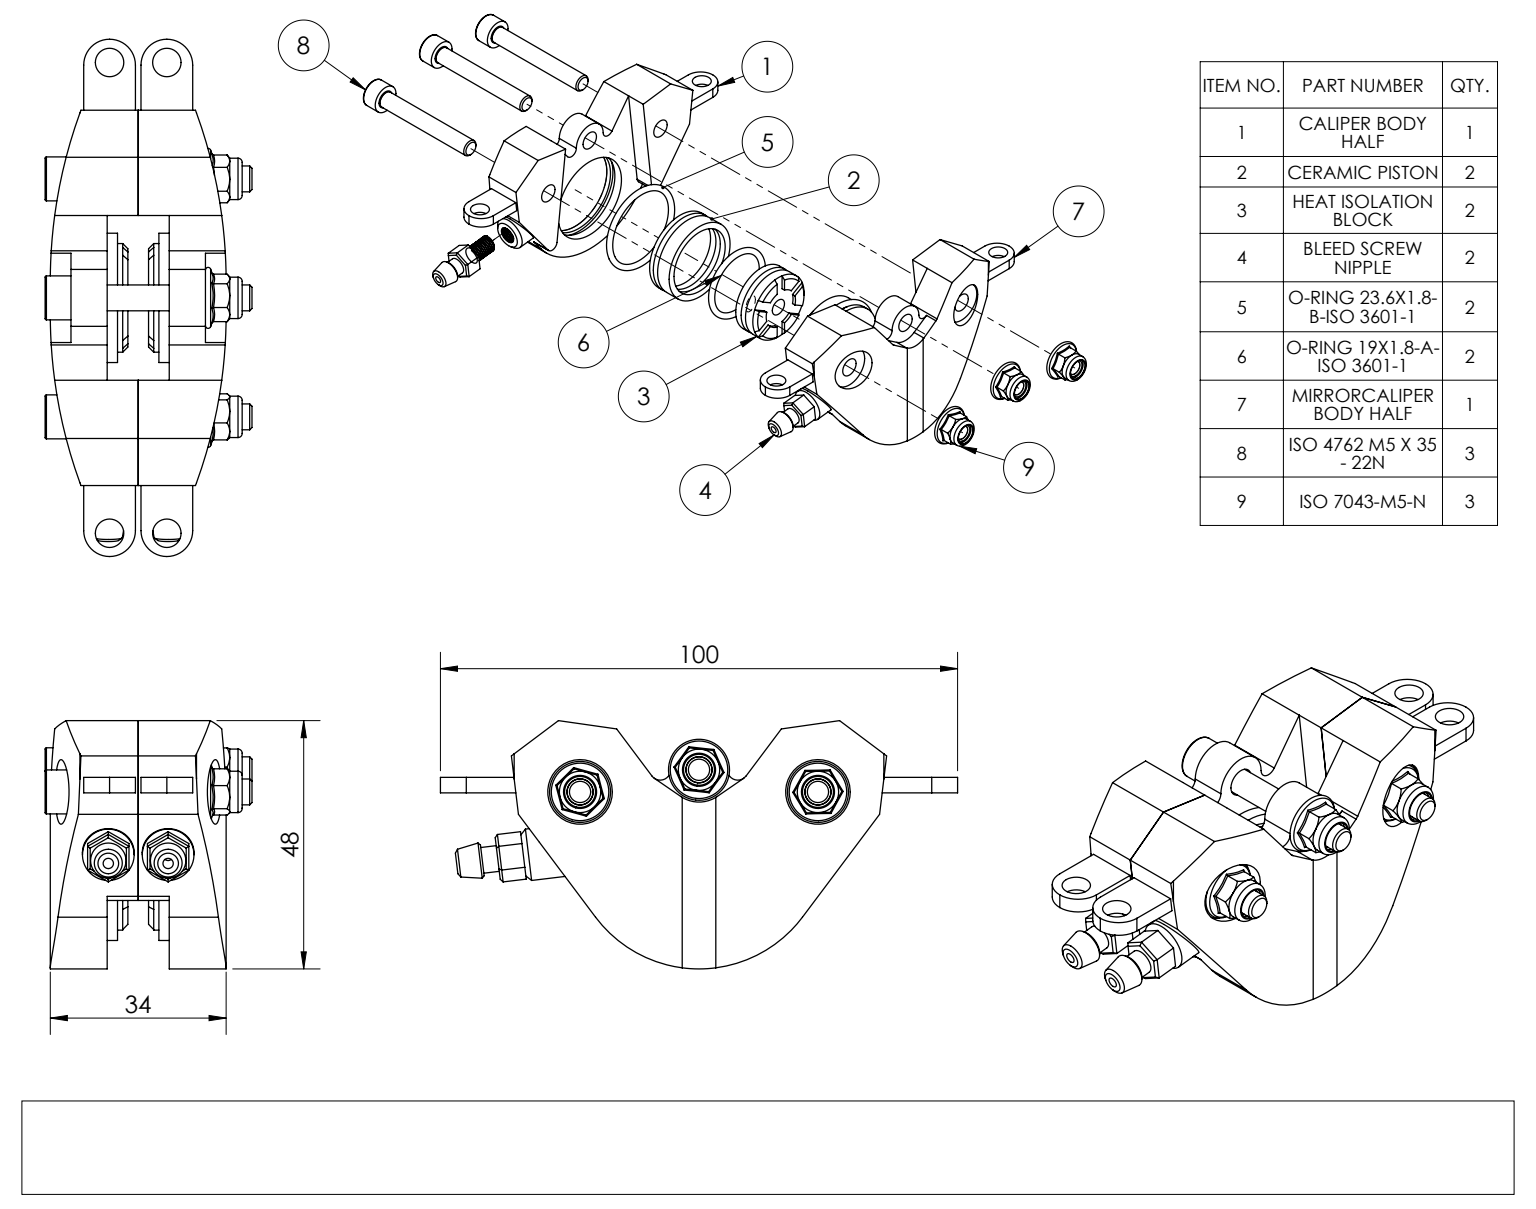
ISO-10303-21;
HEADER;
FILE_DESCRIPTION (('STEP AP214'),
    '1' );
FILE_NAME ('BR-592',
    '2026-09-24T10:28:59',
    ( '' ),
    ( '' ),
    'SwSTEP 2.0',
    'SolidWorks 2026',
    '' );
FILE_SCHEMA (( 'AUTOMOTIVE_DESIGN' ));
ENDSEC;

DATA;
#1 = DIRECTION ( 'NONE',  ( 0.000000000000000000, 0.000000000000000000, 1.000000000000000000 ) ) ;
#2 = CARTESIAN_POINT ( 'NONE',  ( 28.76238721243587193, -5.825490297734302381, -3.627061608673667781 ) ) ;
#3 = CARTESIAN_POINT ( 'NONE',  ( 28.60033944477555323, -4.591072787911525843, -8.283357778048662468 ) ) ;
#4 = FACE_OUTER_BOUND ( 'NONE', #16848, .T. ) ;
#5 = LINE ( 'NONE', #2469, #13948 ) ;
#6 = EDGE_CURVE ( 'NONE', #16160, #8560, #10428, .T. ) ;
#7 = CARTESIAN_POINT ( 'NONE',  ( 27.21934464581372737, -3.303641803799556964, -8.283357778048658915 ) ) ;
#8 = CARTESIAN_POINT ( 'NONE',  ( 31.38469755857769528, -2.374701023479507178, -4.705209693361161349 ) ) ;
#9 = CARTESIAN_POINT ( 'NONE',  ( -4.281152949374567029, -4.203775615332181914, -2.000000000000000000 ) ) ;
#10 = DIRECTION ( 'NONE',  ( -0.1196152422706611984, 0.9928203230275510771, 0.000000000000000000 ) ) ;
#11 = CARTESIAN_POINT ( 'NONE',  ( 0.5636734750061580534, 4.293365120987025385, -3.231543764079864101 ) ) ;
#12 = CARTESIAN_POINT ( 'NONE',  ( -4.140405595019059248, -2.228337868678524458, -3.386887224136967411 ) ) ;
#13 = VECTOR ( 'NONE', #4443, 1000.000000000000000 ) ;
#14 = EDGE_CURVE ( 'NONE', #9007, #1609, #16081, .T. ) ;
#15 =( GEOMETRIC_REPRESENTATION_CONTEXT ( 3 ) GLOBAL_UNCERTAINTY_ASSIGNED_CONTEXT ( ( #3731 ) ) GLOBAL_UNIT_ASSIGNED_CONTEXT ( ( #3713, #4977, #14697 ) ) REPRESENTATION_CONTEXT ( 'NONE', 'WORKASPACE' ) );
#16 = CARTESIAN_POINT ( 'NONE',  ( 29.62036837594175154, -3.214238380052812261, -3.627061608673662896 ) ) ;
#17 = EDGE_CURVE ( 'NONE', #16386, #12240, #657, .T. ) ;
#18 = ORIENTED_EDGE ( 'NONE', *, *, #8443, .T. ) ;
#19 = AXIS2_PLACEMENT_3D ( 'NONE', #16442, #1032, #9441 ) ;
#20 = CIRCLE ( 'NONE', #5504, 10.50000000000000000 ) ;
#21 = CARTESIAN_POINT ( 'NONE',  ( 32.63137222500256485, -6.623491938275930302, -6.453230759126470595 ) ) ;
#22 = CARTESIAN_POINT ( 'NONE',  ( 30.63309003953906995, -6.864245478665264244, -5.783357778048663356 ) ) ;
#23 = ORIENTED_EDGE ( 'NONE', *, *, #13213, .T. ) ;
#24 = DIRECTION ( 'NONE',  ( 0.000000000000000000, 0.000000000000000000, 1.000000000000000000 ) ) ;
#25 = ORIENTED_EDGE ( 'NONE', *, *, #5037, .F. ) ;
#26 = CARTESIAN_POINT ( 'NONE',  ( 30.41294626588012306, -6.253601060580800564, -6.861505862736167138 ) ) ;
#27 = EDGE_CURVE ( 'NONE', #7462, #10575, #2062, .T. ) ;
#28 = CYLINDRICAL_SURFACE ( 'NONE', #14824, 2.749999999999992006 ) ;
#29 = VERTEX_POINT ( 'NONE', #10521 ) ;
#30 = CARTESIAN_POINT ( 'NONE',  ( 26.73899421642883567, -2.634607751922174224, -4.533357778048659803 ) ) ;
#31 = VECTOR ( 'NONE', #7104, 1000.000000000000114 ) ;
#32 = CARTESIAN_POINT ( 'NONE',  ( 29.39961944441754227, -3.040961747597316744, 8.283357778048666020 ) ) ;
#33 = FACE_OUTER_BOUND ( 'NONE', #10742, .T. ) ;
#34 = CONICAL_SURFACE ( 'NONE', #10154, 3.500000000000004885, 0.1745329251994333364 ) ;
#35 = CARTESIAN_POINT ( 'NONE',  ( 26.41562710823574278, -3.600346414165641828, -7.939653947423660263 ) ) ;
#36 = EDGE_LOOP ( 'NONE', ( #1932, #7211, #3460, #1817 ) ) ;
#37 = CARTESIAN_POINT ( 'NONE',  ( 16.95685998530892746, -17.86641812890577796, -16.00584995567978908 ) ) ;
#38 = ORIENTED_EDGE ( 'NONE', *, *, #3823, .T. ) ;
#39 = CONICAL_SURFACE ( 'NONE', #2378, 9.500000000000001776, 0.7853981633974465026 ) ;
#40 = CARTESIAN_POINT ( 'NONE',  ( 27.63266882139180680, -2.199775856772564708, 5.783357778048668685 ) ) ;
#41 = CARTESIAN_POINT ( 'NONE',  ( 19.91592223102268733, -21.66952118561269458, 15.52717098632164117 ) ) ;
#42 = AXIS2_PLACEMENT_3D ( 'NONE', #3726, #1281, #2807 ) ;
#43 = VERTEX_POINT ( 'NONE', #14629 ) ;
#44 = VECTOR ( 'NONE', #8259, 1000.000000000000227 ) ;
#45 = CARTESIAN_POINT ( 'NONE',  ( 31.12210306526553083, -4.287250072544045665, 3.283357778048664244 ) ) ;
#46 = DIRECTION ( 'NONE',  ( 0.000000000000000000, 1.000000000000000000, 0.000000000000000000 ) ) ;
#47 = EDGE_CURVE ( 'NONE', #1330, #15856, #15716, .T. ) ;
#48 = ORIENTED_EDGE ( 'NONE', *, *, #12351, .T. ) ;
#49 = CARTESIAN_POINT ( 'NONE',  ( 33.55383270609817714, -5.448088258586239796, -3.283357778048667797 ) ) ;
#50 = CARTESIAN_POINT ( 'NONE',  ( 29.97942892559193950, -4.424919740341219487, -3.627061608673664672 ) ) ;
#51 = VECTOR ( 'NONE', #5337, 1000.000000000000000 ) ;
#52 = FACE_OUTER_BOUND ( 'NONE', #13800, .T. ) ;
#53 = CARTESIAN_POINT ( 'NONE',  ( -7.511572993685817836E-16, -4.618802153517020059, -3.133295621305386636 ) ) ;
#54 = PRESENTATION_STYLE_ASSIGNMENT (( #17863 ) ) ;
#55 = CARTESIAN_POINT ( 'NONE',  ( 0.000000000000000000, 0.000000000000000000, 0.000000000000000000 ) ) ;
#56 = CARTESIAN_POINT ( 'NONE',  ( 28.75786045390062995, -2.691183018653962034, 4.705209693361167567 ) ) ;
#57 = CARTESIAN_POINT ( 'NONE',  ( -15.92260893619738837, -28.39189527176317540, 12.00000000000000000 ) ) ;
#58 = CARTESIAN_POINT ( 'NONE',  ( 23.00000000000000000, -16.21813761408365195, 0.000000000000000000 ) ) ;
#59 = DIRECTION ( 'NONE',  ( 0.000000000000000000, 0.000000000000000000, 1.000000000000000000 ) ) ;
#60 = VERTEX_POINT ( 'NONE', #9170 ) ;
#61 = AXIS2_PLACEMENT_3D ( 'NONE', #16473, #4043, #10648 ) ;
#62 = CIRCLE ( 'NONE', #4991, 10.50000000000000000 ) ;
#63 = VERTEX_POINT ( 'NONE', #7643 ) ;
#64 = CARTESIAN_POINT ( 'NONE',  ( 27.60205212784272177, -2.830435096530727446, 6.861505862736165362 ) ) ;
#65 = CARTESIAN_POINT ( 'NONE',  ( 27.46709037723411839, -6.908327297984874882, 7.033357778048657138 ) ) ;
#66 = ORIENTED_EDGE ( 'NONE', *, *, #7774, .T. ) ;
#67 = CARTESIAN_POINT ( 'NONE',  ( 26.37178701114681800, -2.351687214456304797, 5.783357778048668685 ) ) ;
#68 = ORIENTED_EDGE ( 'NONE', *, *, #11555, .T. ) ;
#69 = DIRECTION ( 'NONE',  ( 0.5000000000000038858, 0.8660254037844363761, 0.000000000000000000 ) ) ;
#70 = CARTESIAN_POINT ( 'NONE',  ( 26.01652455409633902, -4.902371455920928156, -5.783357778048663356 ) ) ;
#71 = DIRECTION ( 'NONE',  ( 1.000000000000000000, 0.000000000000000000, 0.000000000000000000 ) ) ;
#72 = CARTESIAN_POINT ( 'NONE',  ( 25.86833963875586306, -3.039313213345869791, -4.705209693361160461 ) ) ;
#73 = CARTESIAN_POINT ( 'NONE',  ( 0.000000000000000000, 0.000000000000000000, -2.000000000000000000 ) ) ;
#75 = ADVANCED_FACE ( 'NONE', ( #15989 ), #17272, .F. ) ;
#74 = CARTESIAN_POINT ( 'NONE',  ( 29.12189622942009493, -1.620608325512071568, -5.783357778048658027 ) ) ;
#76 = CARTESIAN_POINT ( 'NONE',  ( 31.70371634254663817, -2.036456781249897485, -4.533357778048659803 ) ) ;
#77 = CIRCLE ( 'NONE', #17181, 2.000000000000001776 ) ;
#78 = CARTESIAN_POINT ( 'NONE',  ( 16.79147592569384173, -15.38964587861223166, -16.02981638571824163 ) ) ;
#79 = CARTESIAN_POINT ( 'NONE',  ( 30.08145424927873535, -6.930706697444451336, 5.783357778048664244 ) ) ;
#80 = CIRCLE ( 'NONE', #3851, 6.000000000000000888 ) ;
#81 = CARTESIAN_POINT ( 'NONE',  ( 29.62036837594175154, -3.214238380052812261, -3.627061608673662896 ) ) ;
#82 = VERTEX_POINT ( 'NONE', #13166 ) ;
#83 = EDGE_CURVE ( 'NONE', #825, #4804, #12452, .T. ) ;
#84 = CARTESIAN_POINT ( 'NONE',  ( 27.88665588685489993, -3.423116496867954162, -3.627061608673662008 ) ) ;
#85 = EDGE_LOOP ( 'NONE', ( #16844, #9736, #6237, #10207 ) ) ;
#86 = CARTESIAN_POINT ( 'NONE',  ( 0.000000000000000000, 0.000000000000000000, -4.700000000000000178 ) ) ;
#87 = EDGE_LOOP ( 'NONE', ( #1855, #1887, #10424, #16720 ) ) ;
#88 = ORIENTED_EDGE ( 'NONE', *, *, #6884, .F. ) ;
#89 = ORIENTED_EDGE ( 'NONE', *, *, #2806, .T. ) ;
#90 = CARTESIAN_POINT ( 'NONE',  ( 28.10549950023367316, -2.142809097641162897, 5.783357778048668685 ) ) ;
#91 = CARTESIAN_POINT ( 'NONE',  ( 26.87106449706838873, -6.053357334259913181, -3.627061608673667781 ) ) ;
#92 = DIRECTION ( 'NONE',  ( 0.000000000000000000, 0.000000000000000000, 1.000000000000000000 ) ) ;
#93 = CARTESIAN_POINT ( 'NONE',  ( 25.76466184735054910, -2.811881907026620553, -6.248149982130924762 ) ) ;
#94 = CARTESIAN_POINT ( 'NONE',  ( 34.91600907648203389, -11.88801210197604341, -11.56671555609732671 ) ) ;
#95 = CARTESIAN_POINT ( 'NONE',  ( 27.62849893492243325, -6.589071975465733644, -4.705209693361168455 ) ) ;
#96 = CARTESIAN_POINT ( 'NONE',  ( -4.000000000000000000, 2.309401076758501592, -0.4999999999999963363 ) ) ;
#97 = LINE ( 'NONE', #5605, #15979 ) ;
#98 = ADVANCED_FACE ( 'NONE', ( #4634, #14352 ), #12979, .F. ) ;
#99 = CARTESIAN_POINT ( 'NONE',  ( 25.11802603177690330, -16.03270077640482683, -0.5379818257722508434 ) ) ;
#100 = AXIS2_PLACEMENT_3D ( 'NONE', #12940, #16861, #525 ) ;
#101 = CARTESIAN_POINT ( 'NONE',  ( 28.51030546511822195, -6.055733689321201041, -3.283357778048667797 ) ) ;
#102 = AXIS2_PLACEMENT_3D ( 'NONE', #2745, #9523, #13625 ) ;
#103 = CARTESIAN_POINT ( 'NONE',  ( 30.62726312072365431, -1.838986382273682718, -5.783357778048658027 ) ) ;
#104 = CARTESIAN_POINT ( 'NONE',  ( 8.249999999999971578, -6.495190528383328221, -3.000000000000002665 ) ) ;
#105 = CARTESIAN_POINT ( 'NONE',  ( 31.03206908560819954, -5.751910973953721751, 8.283357778048660691 ) ) ;
#106 = EDGE_CURVE ( 'NONE', #16432, #2761, #668, .T. ) ;
#107 = DIRECTION ( 'NONE',  ( 0.000000000000000000, 0.000000000000000000, -1.000000000000000000 ) ) ;
#108 = CARTESIAN_POINT ( 'NONE',  ( 32.89331279191618762, -2.620040694222726785, 3.283357778048666464 ) ) ;
#109 = CARTESIAN_POINT ( 'NONE',  ( 26.84461768998868436, -2.294720455324902542, -5.783357778048658915 ) ) ;
#110 = ORIENTED_EDGE ( 'NONE', *, *, #14522, .T. ) ;
#111 = PLANE ( 'NONE',  #4436 ) ;
#112 = CARTESIAN_POINT ( 'NONE',  ( 0.000000000000000000, 0.000000000000000000, -4.000000000000000000 ) ) ;
#113 = ORIENTED_EDGE ( 'NONE', *, *, #12527, .T. ) ;
#114 = CARTESIAN_POINT ( 'NONE',  ( 31.97277696464621854, -6.702839660918840536, 5.783357778048664244 ) ) ;
#115 = ORIENTED_EDGE ( 'NONE', *, *, #562, .T. ) ;
#116 = CARTESIAN_POINT ( 'NONE',  ( 28.26310972651430120, -2.123820177930694442, -5.783357778048658915 ) ) ;
#117 = CARTESIAN_POINT ( 'NONE',  ( -23.02601376483258022, 3.965314980223224151, 6.000000000000000000 ) ) ;
#118 = VERTEX_POINT ( 'NONE', #924 ) ;
#119 = ORIENTED_EDGE ( 'NONE', *, *, #5679, .T. ) ;
#120 = CARTESIAN_POINT ( 'NONE',  ( 30.15026255541241440, -6.285249260098253465, -4.705209693361168455 ) ) ;
#121 = CARTESIAN_POINT ( 'NONE',  ( 29.19631194059803292, -2.001190877926593004, 6.453230759126469707 ) ) ;
#122 = VERTEX_POINT ( 'NONE', #5078 ) ;
#123 = CARTESIAN_POINT ( 'NONE',  ( 31.90644508241650357, -6.373472726347483963, -7.033357778048666908 ) ) ;
#124 = DIRECTION ( 'NONE',  ( 0.000000000000000000, 0.000000000000000000, -1.000000000000000000 ) ) ;
#125 = ORIENTED_EDGE ( 'NONE', *, *, #6084, .F. ) ;
#126 = CARTESIAN_POINT ( 'NONE',  ( 26.66770885555339987, -3.370103022578743612, 3.283357778048666464 ) ) ;
#127 = ADVANCED_FACE ( 'NONE', ( #4081 ), #12055, .F. ) ;
#128 = LINE ( 'NONE', #15357, #5139 ) ;
#129 = CARTESIAN_POINT ( 'NONE',  ( 27.17934203385504333, -30.00000000000000355, 0.000000000000000000 ) ) ;
#130 = DIRECTION ( 'NONE',  ( 0.8660254037844432595, 0.4999999999999921174, 0.000000000000000000 ) ) ;
#131 = VERTEX_POINT ( 'NONE', #5429 ) ;
#132 = CARTESIAN_POINT ( 'NONE',  ( 31.27600417729400917, -6.449428405189353342, 4.533357778048659803 ) ) ;
#133 = VERTEX_POINT ( 'NONE', #2641 ) ;
#134 = CARTESIAN_POINT ( 'NONE',  ( -3.248936832696171617, 7.999999999999989342, -17.00000000000000000 ) ) ;
#135 = ORIENTED_EDGE ( 'NONE', *, *, #7750, .F. ) ;
#136 = CARTESIAN_POINT ( 'NONE',  ( 0.000000000000000000, 0.000000000000000000, 0.000000000000000000 ) ) ;
#137 = EDGE_CURVE ( 'NONE', #13969, #14024, #12150, .T. ) ;
#138 = CARTESIAN_POINT ( 'NONE',  ( 27.02867472334902033, -6.034368414549446058, -3.627061608673668225 ) ) ;
#139 = CARTESIAN_POINT ( 'NONE',  ( 33.14105852333657509, -6.224726188408045147, -4.533357778048668685 ) ) ;
#140 = CARTESIAN_POINT ( 'NONE',  ( -2.016448651773435938E-27, -20.49999999999999645, -13.00000000000000178 ) ) ;
#141 = CARTESIAN_POINT ( 'NONE',  ( 31.03206908560819954, -5.751910973953721751, -3.283357778048667797 ) ) ;
#142 = CARTESIAN_POINT ( 'NONE',  ( 30.01874226414561875, -2.539271660970221944, 4.705209693361167567 ) ) ;
#143 = CARTESIAN_POINT ( 'NONE',  ( 0.000000000000000000, 0.000000000000000000, -3.000000000000000000 ) ) ;
#144 = CARTESIAN_POINT ( 'NONE',  ( 30.66050125466253107, -2.889050389913576655, -3.283357778048662023 ) ) ;
#145 = CARTESIAN_POINT ( 'NONE',  ( 31.55553118839817728, -4.235030543236534939, 3.627061608673664228 ) ) ;
#146 = ORIENTED_EDGE ( 'NONE', *, *, #8317, .T. ) ;
#147 = ADVANCED_FACE ( 'NONE', ( #12333 ), #17898, .T. ) ;
#148 = EDGE_LOOP ( 'NONE', ( #1703, #3321, #10614, #8753 ) ) ;
#149 = CARTESIAN_POINT ( 'NONE',  ( 28.24571643650507369, -4.633797857156355171, 3.627061608673664228 ) ) ;
#150 = CARTESIAN_POINT ( 'NONE',  ( 31.92138306490751987, -2.737139032229836566, -3.283357778048662023 ) ) ;
#151 = DIRECTION ( 'NONE',  ( 0.000000000000000000, 0.000000000000000000, -1.000000000000000000 ) ) ;
#152 = ORIENTED_EDGE ( 'NONE', *, *, #13921, .T. ) ;
#153 = CARTESIAN_POINT ( 'NONE',  ( 27.88665588685489993, -3.423116496867954162, 7.939653947423662927 ) ) ;
#154 = ORIENTED_EDGE ( 'NONE', *, *, #5892, .F. ) ;
#155 = ORIENTED_EDGE ( 'NONE', *, *, #14955, .F. ) ;
#156 = CYLINDRICAL_SURFACE ( 'NONE', #2297, 2.749999999999992006 ) ;
#157 = FACE_OUTER_BOUND ( 'NONE', #4677, .T. ) ;
#158 = DIRECTION ( 'NONE',  ( -1.000000000000000000, -0.000000000000000000, -0.000000000000000000 ) ) ;
#159 = B_SPLINE_CURVE_WITH_KNOTS ( 'NONE', 3,
 ( #17069, #3694, #6069, #7869 ),
 .UNSPECIFIED., .F., .F.,
 ( 4, 4 ),
 ( 0.000000000000000000, 0.0006487028241592422868 ),
 .UNSPECIFIED. ) ;
#160 = CARTESIAN_POINT ( 'NONE',  ( 26.52522735095806894, -6.721994413439005278, -4.705209693361169343 ) ) ;
#161 = CARTESIAN_POINT ( 'NONE',  ( 33.50243880635947846, -1.482387629897225390, -5.783357778048663356 ) ) ;
#162 = CARTESIAN_POINT ( 'NONE',  ( 27.92859066579839222, -3.218191664895003967, -8.283357778048658915 ) ) ;
#163 = CARTESIAN_POINT ( 'NONE',  ( 28.29479612530171551, -12.89112598890823946, -13.63906826012424922 ) ) ;
#164 = DIRECTION ( 'NONE',  ( 1.000000000000000000, 0.000000000000000000, 0.000000000000000000 ) ) ;
#165 =( LENGTH_UNIT ( ) NAMED_UNIT ( * ) SI_UNIT ( .MILLI., .METRE. ) );
#166 = CARTESIAN_POINT ( 'NONE',  ( 31.30154412293507349, -3.011689903141150815, -7.939653947423660263 ) ) ;
#167 = EDGE_LOOP ( 'NONE', ( #6855, #14181, #5684, #15430, #4604, #9201, #7856, #12095, #740, #13288, #12189, #5777, #2747, #13452, #12769, #7783, #17571, #8793, #8444, #8354, #17242, #15258, #14922, #10965, #8092, #5094, #9620, #17228, #363 ) ) ;
#168 = CARTESIAN_POINT ( 'NONE',  ( 28.28502977505876359, -2.748149777785362957, -6.861505862736158257 ) ) ;
#169 = FACE_BOUND ( 'NONE', #9729, .T. ) ;
#170 = ORIENTED_EDGE ( 'NONE', *, *, #10749, .T. ) ;
#171 = ORIENTED_EDGE ( 'NONE', *, *, #13786, .T. ) ;
#172 = VERTEX_POINT ( 'NONE', #5336 ) ;
#173 = ADVANCED_FACE ( 'NONE', ( #9510 ), #13344, .F. ) ;
#174 = ORIENTED_EDGE ( 'NONE', *, *, #13419, .F. ) ;
#175 = CARTESIAN_POINT ( 'NONE',  ( 30.04066231269008469, -3.163601260824890904, 3.627061608673666449 ) ) ;
#176 = CARTESIAN_POINT ( 'NONE',  ( 25.99795558426325215, -4.648046406214923820, -3.627061608673664228 ) ) ;
#177 = FACE_OUTER_BOUND ( 'NONE', #11097, .T. ) ;
#178 = DIRECTION ( 'NONE',  ( 0.000000000000000000, 0.000000000000000000, -1.000000000000000000 ) ) ;
#179 = CARTESIAN_POINT ( 'NONE',  ( 29.35841309260160159, -6.680460261459264970, -4.533357778048668685 ) ) ;
#180 = CARTESIAN_POINT ( 'NONE',  ( 29.51982165028991645, -6.361204938940122844, -4.705209693361168455 ) ) ;
#181 = CARTESIAN_POINT ( 'NONE',  ( 31.97277696464621854, -6.702839660918840536, -5.783357778048663356 ) ) ;
#182 = EDGE_CURVE ( 'NONE', #5342, #17048, #16351, .T. ) ;
#183 = DIRECTION ( 'NONE',  ( 1.000000000000000000, 0.000000000000000000, 0.000000000000000000 ) ) ;
#184 = ORIENTED_EDGE ( 'NONE', *, *, #3114, .F. ) ;
#185 = CARTESIAN_POINT ( 'NONE',  ( -27.17934203385504333, -30.00000000000000355, -13.93658524716016878 ) ) ;
#186 = CARTESIAN_POINT ( 'NONE',  ( 29.18195272205665347, -2.340279496617377664, -4.533357778048659803 ) ) ;
#187 =( BOUNDED_SURFACE ( )  B_SPLINE_SURFACE ( 3, 2, ( 
 ( #15565, #5853, #6132 ),
 ( #7149, #10017, #8682 ),
 ( #15660, #7420, #17130 ),
 ( #8776, #4680, #7501 ),
 ( #518, #1619, #4589 ),
 ( #14209, #7333, #249 ) ),
 .UNSPECIFIED., .F., .F., .T. ) 
 B_SPLINE_SURFACE_WITH_KNOTS ( ( 4, 2, 4 ),
 ( 3, 3 ),
 ( 0.02018906359535397113, 0.02264947622839649788, 0.02510988886143902810 ),
 ( 0.000000000000000000, 1.000000000000000000 ),
 .UNSPECIFIED. ) 
 GEOMETRIC_REPRESENTATION_ITEM ( )  RATIONAL_B_SPLINE_SURFACE ( (
 ( 1.000000000000000000, 0.8047781357041529082, 1.000000000000000000),
 ( 1.000000000000000000, 0.8123775905861528868, 1.000000000000000000),
 ( 1.000000000000000000, 0.8190671519372876297, 1.000000000000000000),
 ( 1.000000000000000000, 0.8192352278312100555, 1.000000000000000000),
 ( 1.000000000000000000, 0.8126131206996280998, 1.000000000000000000),
 ( 1.000000000000000000, 0.8047712494894333490, 1.000000000000000000) ) ) 
 REPRESENTATION_ITEM ( '' )  SURFACE ( )  );
#188 = CARTESIAN_POINT ( 'NONE',  ( 31.41114436565740320, -6.133337902414513820, -4.705209693361168455 ) ) ;
#189 = FACE_OUTER_BOUND ( 'NONE', #16988, .T. ) ;
#190 = DIRECTION ( 'NONE',  ( -1.000000000000000000, 0.000000000000000000, 0.000000000000000000 ) ) ;
#191 = CARTESIAN_POINT ( 'NONE',  ( 39.34669483983374505, -6.862522726337943801, -6.650911402496568314 ) ) ;
#192 = CARTESIAN_POINT ( 'NONE',  ( 31.59864285835955400, -2.049116061056871274, 4.533357778048667797 ) ) ;
#193 = CARTESIAN_POINT ( 'NONE',  ( 27.60205212784272177, -2.830435096530727446, -4.705209693361161349 ) ) ;
#194 = EDGE_CURVE ( 'NONE', #11172, #2496, #13438, .T. ) ;
#195 = ORIENTED_EDGE ( 'NONE', *, *, #15251, .T. ) ;
#196 = CARTESIAN_POINT ( 'NONE',  ( 26.87859896403794835, -7.316587507915443211, 5.113484796970851676 ) ) ;
#197 = DIRECTION ( 'NONE',  ( -1.000000000000000000, 0.000000000000000000, 0.000000000000000000 ) ) ;
#198 = ORIENTED_EDGE ( 'NONE', *, *, #5351, .T. ) ;
#199 = DIRECTION ( 'NONE',  ( 0.000000000000000000, -1.000000000000000000, 0.000000000000000000 ) ) ;
#200 = EDGE_LOOP ( 'NONE', ( #3718, #1302, #8199, #7677, #6005, #1633 ) ) ;
#201 = EDGE_CURVE ( 'NONE', #3274, #13752, #311, .T. ) ;
#202 = DIRECTION ( 'NONE',  ( -1.000000000000000000, 0.000000000000000000, 0.000000000000000000 ) ) ;
#203 = CARTESIAN_POINT ( 'NONE',  ( 3.248936832696173393, 17.78798921770683350, 17.00000000000000000 ) ) ;
#204 = ORIENTED_EDGE ( 'NONE', *, *, #11417, .T. ) ;
#205 = VECTOR ( 'NONE', #5367, 1000.000000000000227 ) ;
#207 = EDGE_LOOP ( 'NONE', ( #11422, #8377, #17595, #13814 ) ) ;
#206 =( BOUNDED_CURVE ( )  B_SPLINE_CURVE ( 2, ( #6130, #9128, #12848, #438, #15840, #5943, #14486, #14392, #13119 ),
 .UNSPECIFIED., .F., .T. ) 
 B_SPLINE_CURVE_WITH_KNOTS ( ( 3, 2, 2, 2, 3 ),
 ( 0.6730769230769231282, 0.6794871794871795156, 0.6923076923076922906, 0.7051282051282051766, 0.7115384615384615641 ),
 .UNSPECIFIED. ) 
 CURVE ( )  GEOMETRIC_REPRESENTATION_ITEM ( )  RATIONAL_B_SPLINE_CURVE ( ( 0.9330127018922192983, 0.9330127018922198534, 1.000000000000000000, 0.8660254037844387076, 1.000000000000000000, 0.8660254037844387076, 1.000000000000000000, 0.9330127018922194093, 0.9330127018922194093 ) ) 
 REPRESENTATION_ITEM ( '' )  );
#208 = CARTESIAN_POINT ( 'NONE',  ( 28.86293393808771057, -2.678523738846987357, -4.705209693361161349 ) ) ;
#209 = CARTESIAN_POINT ( 'NONE',  ( 42.20068782821381603, -5.470578387159230616, -5.783357778048662468 ) ) ;
#210 = CARTESIAN_POINT ( 'NONE',  ( 32.57506351453486815, -6.630276025878011126, 6.453230759126467042 ) ) ;
#211 = ORIENTED_EDGE ( 'NONE', *, *, #16657, .F. ) ;
#212 = CARTESIAN_POINT ( 'NONE',  ( 33.55383270609817714, -5.448088258586239796, -3.283357778048667797 ) ) ;
#213 = ORIENTED_EDGE ( 'NONE', *, *, #17178, .T. ) ;
#214 = CARTESIAN_POINT ( 'NONE',  ( 31.61111609099199171, -1.710254666422835745, -5.783357778048662468 ) ) ;
#215 = CARTESIAN_POINT ( 'NONE',  ( 33.17547354829333273, -5.293800545841212291, 7.939653947423658487 ) ) ;
#216 = AXIS2_PLACEMENT_3D ( 'NONE', #2816, #4451, #10954 ) ;
#217 = AXIS2_PLACEMENT_3D ( 'NONE', #13648, #13735, #1318 ) ;
#218 = EDGE_CURVE ( 'NONE', #17680, #17749, #13335, .T. ) ;
#219 = VECTOR ( 'NONE', #12447, 1000.000000000000000 ) ;
#220 = DIRECTION ( 'NONE',  ( 0.9928203230275512992, 0.1196152422706610319, 9.614813431917826478E-17 ) ) ;
#221 = DIRECTION ( 'NONE',  ( 0.9899494936611662466, -0.1414213562373111965, 0.000000000000000000 ) ) ;
#222 = CARTESIAN_POINT ( 'NONE',  ( -25.11802603177690330, -19.03270077640482683, -10.53798182577225084 ) ) ;
#223 = ORIENTED_EDGE ( 'NONE', *, *, #9237, .T. ) ;
#224 = CARTESIAN_POINT ( 'NONE',  ( 28.67914455963771303, -4.581578327848842669, 3.283357778048664244 ) ) ;
#225 = VERTEX_POINT ( 'NONE', #1017 ) ;
#226 = CARTESIAN_POINT ( 'NONE',  ( 26.92924972366625980, -7.310485091653801781, 5.783357778048669573 ) ) ;
#227 = VERTEX_POINT ( 'NONE', #1284 ) ;
#228 = CARTESIAN_POINT ( 'NONE',  ( 45.50000000000000000, -16.03270077640482683, 5.537981825772250843 ) ) ;
#229 = CARTESIAN_POINT ( 'NONE',  ( 25.93488947238681774, -5.606027099510431988, -7.939653947423663816 ) ) ;
#230 = ADVANCED_FACE ( 'NONE', ( #6542 ), #5163, .T. ) ;
#231 = CARTESIAN_POINT ( 'NONE',  ( 31.74131510559286085, -5.666460835049168310, -3.283357778048667797 ) ) ;
#232 = DIRECTION ( 'NONE',  ( 0.000000000000000000, 0.000000000000000000, -1.000000000000000000 ) ) ;
#233 = APPLICATION_PROTOCOL_DEFINITION ( 'draft international standard', 'automotive_design', 1998, #5728 ) ;
#234 = DIRECTION ( 'NONE',  ( 1.000000000000000000, 0.000000000000000000, 0.000000000000000000 ) ) ;
#235 =( GEOMETRIC_REPRESENTATION_CONTEXT ( 3 ) GLOBAL_UNCERTAINTY_ASSIGNED_CONTEXT ( ( #1389 ) ) GLOBAL_UNIT_ASSIGNED_CONTEXT ( ( #897, #4698, #14414 ) ) REPRESENTATION_CONTEXT ( 'NONE', 'WORKASPACE' ) );
#236 = DIRECTION ( 'NONE',  ( 0.000000000000000000, 0.000000000000000000, 1.000000000000000000 ) ) ;
#237 = CARTESIAN_POINT ( 'NONE',  ( 31.70371634254663817, -2.036456781249897485, 7.033357778048666020 ) ) ;
#238 = CARTESIAN_POINT ( 'NONE',  ( 29.52399153675929355, -1.971908820246954130, 5.783357778048668685 ) ) ;
#239 = ORIENTED_EDGE ( 'NONE', *, *, #8844, .T. ) ;
#240 = VECTOR ( 'NONE', #8984, 1000.000000000000000 ) ;
#241 = ORIENTED_EDGE ( 'NONE', *, *, #27, .F. ) ;
#242 = CARTESIAN_POINT ( 'NONE',  ( 29.49337484321020497, -2.602568060005117090, 6.861505862736165362 ) ) ;
#243 = DIRECTION ( 'NONE',  ( 0.000000000000000000, 0.000000000000000000, -1.000000000000000000 ) ) ;
#244 = CARTESIAN_POINT ( 'NONE',  ( 26.00347982711925710, -2.723222710571018279, -7.033357778048658027 ) ) ;
#245 = ORIENTED_EDGE ( 'NONE', *, *, #2656, .T. ) ;
#246 = CARTESIAN_POINT ( 'NONE',  ( 27.12922144900085186, -2.887401855662130146, 6.861505862736166250 ) ) ;
#247 = DIRECTION ( 'NONE',  ( -0.9928203230275512992, -0.1196152422706610319, -9.614813431917826478E-17 ) ) ;
#248 = AXIS2_PLACEMENT_3D ( 'NONE', #3421, #10388, #11749 ) ;
#249 = CARTESIAN_POINT ( 'NONE',  ( -4.211405941597130109, -2.460460478483078361, -3.451298436431160077 ) ) ;
#250 = CARTESIAN_POINT ( 'NONE',  ( 0.000000000000000000, 0.000000000000000000, -9.600000000000001421 ) ) ;
#251 = CIRCLE ( 'NONE', #10368, 10.50000000000000000 ) ;
#252 = CYLINDRICAL_SURFACE ( 'NONE', #8155, 1.000000000000000000 ) ;
#253 = CARTESIAN_POINT ( 'NONE',  ( 0.000000000000000000, 0.000000000000000000, -9.600000000000001421 ) ) ;
#254 = VERTEX_POINT ( 'NONE', #16603 ) ;
#255 = CARTESIAN_POINT ( 'NONE',  ( 31.11087420047036289, -5.742416513891037688, -3.283357778048667797 ) ) ;
#256 = ADVANCED_FACE ( 'NONE', ( #8427, #1643 ), #16881, .T. ) ;
#257 = CARTESIAN_POINT ( 'NONE',  ( 19.43845002722867221, 2.988003976273735596, -6.000000000000000000 ) ) ;
#258 = CARTESIAN_POINT ( 'NONE',  ( 0.000000000000000000, 0.000000000000000000, -4.394516984716110741 ) ) ;
#259 = APPLICATION_PROTOCOL_DEFINITION ( 'draft international standard', 'automotive_design', 1998, #17836 ) ;
#260 = CARTESIAN_POINT ( 'NONE',  ( 32.77257290155422709, -2.834459985843461816, -3.627061608673662896 ) ) ;
#261 = VECTOR ( 'NONE', #7073, 1000.000000000000227 ) ;
#262 = CARTESIAN_POINT ( 'NONE',  ( 25.76466184735054910, -2.811881907026620553, -6.248149982130924762 ) ) ;
#263 = CARTESIAN_POINT ( 'NONE',  ( -9.099998387031003944, -19.29508120620799616, -16.81964500401478091 ) ) ;
#264 = CIRCLE ( 'NONE', #10381, 4.250000000000000000 ) ;
#265 = EDGE_CURVE ( 'NONE', #1659, #12087, #14509, .T. ) ;
#266 = ORIENTED_EDGE ( 'NONE', *, *, #8133, .F. ) ;
#267 = EDGE_LOOP ( 'NONE', ( #17915, #6076 ) ) ;
#268 = CARTESIAN_POINT ( 'NONE',  ( 27.75549246765397271, -7.200742295513424374, 5.783357778048658915 ) ) ;
#269 = DIRECTION ( 'NONE',  ( -0.1196152422706618645, 0.9928203230275510771, 0.000000000000000000 ) ) ;
#270 = CARTESIAN_POINT ( 'NONE',  ( 23.00000000000000000, -16.21813761408365195, -13.00000000000000178 ) ) ;
#271 = PLANE ( 'NONE',  #2587 ) ;
#272 = CARTESIAN_POINT ( 'NONE',  ( 0.000000000000000000, -1.178949249685218081, -2.041999999999998039 ) ) ;
#273 = CARTESIAN_POINT ( 'NONE',  ( 30.04066231269008469, -3.163601260824890904, -7.939653947423660263 ) ) ;
#274 = CARTESIAN_POINT ( 'NONE',  ( 29.26075783691881682, -2.330785036554694489, -4.533357778048659803 ) ) ;
#275 = CARTESIAN_POINT ( 'NONE',  ( 26.01652455409633902, -4.902371455920926380, -5.783357778048663356 ) ) ;
#276 = VECTOR ( 'NONE', #9402, 1000.000000000000227 ) ;
#277 = LINE ( 'NONE', #4351, #8745 ) ;
#278 = EDGE_CURVE ( 'NONE', #1298, #15606, #15319, .T. ) ;
#279 = UNCERTAINTY_MEASURE_WITH_UNIT (LENGTH_MEASURE( 1.000000000000000082E-05 ), #1494, 'distance_accuracy_value', 'NONE');
#280 = CARTESIAN_POINT ( 'NONE',  ( 5.200000000000002842, 0.000000000000000000, 2.500000000000000444 ) ) ;
#281 = ORIENTED_EDGE ( 'NONE', *, *, #15299, .F. ) ;
#282 = CARTESIAN_POINT ( 'NONE',  ( 28.88938074516742205, -6.437160617781993999, -4.705209693361168455 ) ) ;
#283 = LINE ( 'NONE', #14248, #9848 ) ;
#284 = DIRECTION ( 'NONE',  ( 0.9899494936611662466, -0.1414213562373111965, 0.000000000000000000 ) ) ;
#285 = CARTESIAN_POINT ( 'NONE',  ( -15.92260893619738837, -28.39189527176317540, 16.15082599432113142 ) ) ;
#286 = VECTOR ( 'NONE', #8460, 1000.000000000000227 ) ;
#287 = DIRECTION ( 'NONE',  ( -0.1196152422706621005, -0.9928203230275509661, 0.000000000000000000 ) ) ;
#288 = CARTESIAN_POINT ( 'NONE',  ( 31.94023320572814484, -7.096308717197083560, 5.783357778048657138 ) ) ;
#289 = CARTESIAN_POINT ( 'NONE',  ( 26.35439372113758694, -4.861664893681965083, -7.939653947423662039 ) ) ;
#290 = VECTOR ( 'NONE', #14393, 1000.000000000000000 ) ;
#291 = ORIENTED_EDGE ( 'NONE', *, *, #11495, .T. ) ;
#292 = CARTESIAN_POINT ( 'NONE',  ( -35.77680296528374271, -19.03270077640482683, -10.53798182577225084 ) ) ;
#293 = DIRECTION ( 'NONE',  ( 0.9237280213470681067, 0.3830490080632377170, 0.000000000000000000 ) ) ;
#294 = CARTESIAN_POINT ( 'NONE',  ( -19.22778933661430756, -11.21824206523807099, -15.64718775662042560 ) ) ;
#295 = ORIENTED_EDGE ( 'NONE', *, *, #12061, .T. ) ;
#296 = AXIS2_PLACEMENT_3D ( 'NONE', #16194, #10362, #13007 ) ;
#297 =( BOUNDED_SURFACE ( )  B_SPLINE_SURFACE ( 1, 2, ( 
 ( #2861, #15197, #16560, #1329, #12111, #15107, #10908, #4144, #1250, #8037, #10736, #5570, #5480, #9559, #4046, #9474, #17694, #15013, #3878, #2779, #5217, #13662, #9391, #13829, #1416, #14933, #6939, #11088, #13573, #1154, #6676, #12207, #5305, #10826, #2693, #336, #16742, #6022, #9824, #15375, #8767, #5843, #145, #12649, #14022, #4493, #11547, #11262, #1693, #12921, #5748, #3051, #11366, #3136, #7410, #11170, #4404, #1607, #15648, #4314, #16935, #8571, #10007, #14299, #2958, #428, #5933, #1884, #506, #17116, #12739, #4670, #7137, #8487, #15553, #238, #8669, #16841, #5659, #12840, #9919, #14106, #12564, #15469, #11457, #10197, #7226, #15747, #8388, #13920, #14196, #1790, #1516, #17024, #7321, #4578, #10099, #3226, #7049, #17304, #13377, #9199, #6214, #9119, #17215, #7674, #3496, #14476, #4756, #13013, #6492, #10628, #863, #6120, #2156, #13284, #15921, #11732, #7583, #2060, #11648, #10465, #12006, #10281, #14658, #17588, #690, #17503, #15830, #13198, #959, #6395, #2240, #7753, #16026, #11913, #598, #5108, #4841, #7490, #2331, #5027, #3403, #3598, #10549, #7850, #16113, #9026, #3675, #10369, #14577, #14745, #8935, #13110, #775 ),
 ( #8849, #3320, #6302, #11824, #14384, #1966, #17402, #4932, #6566, #5194, #5614, #8440, #5799, #12613, #1562, #11131, #7186, #108, #9454, #13976, #3940, #10715, #13473, #6652, #12182, #1466, #13879, #15330, #11219, #12086, #6994, #16288, #1046, #2491, #3858, #14991, #12696, #2908, #9777, #3012, #192, #9368, #5704, #17673, #9287, #288, #2578, #13552, #4274, #16201, #14909, #7095, #3766, #8014, #14829, #1127, #8347, #17761, #5284, #2414, #16794, #7936, #15427, #12522, #16700, #10801, #16376, #4362, #9872, #14068, #8534, #1651, #4454, #14150, #385, #556, #3281, #14252, #11695, #8897, #1840, #11603, #5893, #10323, #12789, #11315, #17073, #3455, #8813, #16895, #12973, #3180, #17167, #15515, #7370, #13155, #3097, #5977, #14344, #7274, #11414, #6074, #8620, #8985, #4716, #16980, #14528, #7450, #10150, #12886, #2111, #471, #1744, #15790, #735, #11502, #9965, #14430, #6171, #4535, #3365, #17264, #15880, #10055, #7539, #15604, #10242, #2014, #8720, #1931, #4626, #7634, #15700, #13064, #4800, #647, #15980, #10512, #11874, #2379, #3903, #9164, #17550, #10763, #3642, #916, #16157, #1010, #5243, #9079, #2286, #17452, #13517, #14621, #3721 ) ),
 .UNSPECIFIED., .F., .F., .F. ) 
 B_SPLINE_SURFACE_WITH_KNOTS ( ( 2, 2 ),
 ( 3, 2, 2, 2, 2, 2, 2, 2, 2, 2, 2, 2, 2, 2, 2, 2, 2, 2, 2, 2, 2, 2, 2, 2, 2, 2, 2, 2, 2, 2, 2, 2, 2, 2, 2, 2, 2, 2, 2, 2, 2, 2, 2, 2, 2, 2, 2, 2, 2, 2, 2, 2, 2, 2, 2, 2, 2, 2, 2, 2, 2, 2, 2, 2, 2, 2, 2, 2, 2, 2, 2, 2, 2, 2, 2, 2, 2, 3 ),
 ( 0.000000000000000000, 1.000000000000000000 ),
 ( 0.000000000000000000, 0.01282051282051282007, 0.02564102564102564014, 0.03846153846153846367, 0.05128205128205128027, 0.06410256410256409687, 0.07692307692307692735, 0.08974358974358974395, 0.1025641025641025605, 0.1153846153846153910, 0.1282051282051281937, 0.1410256410256410242, 0.1538461538461538547, 0.1666666666666666574, 0.1794871794871794879, 0.1923076923076923184, 0.2051282051282051211, 0.2179487179487179516, 0.2307692307692307820, 0.2435897435897435848, 0.2564102564102563875, 0.2692307692307692180, 0.2820512820512820484, 0.2948717948717948789, 0.3076923076923077094, 0.3205128205128205399, 0.3333333333333333148, 0.3461538461538461453, 0.3589743589743589758, 0.3717948717948718063, 0.3846153846153846367, 0.3974358974358974117, 0.4102564102564102422, 0.4230769230769230727, 0.4358974358974359031, 0.4487179487179487336, 0.4615384615384615641, 0.4743589743589743390, 0.4871794871794871695, 0.5000000000000000000, 0.5128205128205127750, 0.5256410256410256610, 0.5384615384615384359, 0.5512820512820513219, 0.5641025641025640969, 0.5769230769230768718, 0.5897435897435897578, 0.6025641025641025328, 0.6153846153846154188, 0.6282051282051281937, 0.6410256410256410797, 0.6538461538461538547, 0.6666666666666666297, 0.6794871794871795156, 0.6923076923076922906, 0.7051282051282051766, 0.7179487179487179516, 0.7307692307692307265, 0.7435897435897436125, 0.7564102564102563875, 0.7692307692307692735, 0.7820512820512820484, 0.7948717948717948234, 0.8076923076923077094, 0.8205128205128204844, 0.8333333333333333703, 0.8461538461538461453, 0.8589743589743589203, 0.8717948717948718063, 0.8846153846153845812, 0.8974358974358974672, 0.9102564102564102422, 0.9230769230769231282, 0.9358974358974359031, 0.9487179487179486781, 0.9615384615384615641, 0.9690837477411259338, 0.9787745852185372186 ),
 .UNSPECIFIED. ) 
 GEOMETRIC_REPRESENTATION_ITEM ( )  RATIONAL_B_SPLINE_SURFACE ( (
 ( 1.000000000000000000, 0.8660254037844387076, 1.000000000000000000, 0.8660254037844387076, 1.000000000000000000, 0.8660254037844387076, 1.000000000000000000, 0.8660254037844387076, 1.000000000000000000, 0.8660254037844387076, 1.000000000000000000, 0.8660254037844387076, 1.000000000000000000, 0.8660254037844387076, 1.000000000000000000, 0.8660254037844387076, 1.000000000000000000, 0.8660254037844387076, 1.000000000000000000, 0.8660254037844387076, 1.000000000000000000, 0.8660254037844387076, 1.000000000000000000, 0.8660254037844387076, 1.000000000000000000, 0.8660254037844387076, 1.000000000000000000, 0.8660254037844387076, 1.000000000000000000, 0.8660254037844387076, 1.000000000000000000, 0.8660254037844387076, 1.000000000000000000, 0.8660254037844387076, 1.000000000000000000, 0.8660254037844387076, 1.000000000000000000, 0.8660254037844387076, 1.000000000000000000, 0.8660254037844387076, 1.000000000000000000, 0.8660254037844387076, 1.000000000000000000, 0.8660254037844387076, 1.000000000000000000, 0.8660254037844387076, 1.000000000000000000, 0.8660254037844387076, 1.000000000000000000, 0.8660254037844387076, 1.000000000000000000, 0.8660254037844387076, 1.000000000000000000, 0.8660254037844387076, 1.000000000000000000, 0.8660254037844387076, 1.000000000000000000, 0.8660254037844387076, 1.000000000000000000, 0.8660254037844387076, 1.000000000000000000, 0.8660254037844387076, 1.000000000000000000, 0.8660254037844387076, 1.000000000000000000, 0.8660254037844387076, 1.000000000000000000, 0.8660254037844387076, 1.000000000000000000, 0.8660254037844387076, 1.000000000000000000, 0.8660254037844387076, 1.000000000000000000, 0.8660254037844387076, 1.000000000000000000, 0.8660254037844387076, 1.000000000000000000, 0.8660254037844387076, 1.000000000000000000, 0.8660254037844387076, 1.000000000000000000, 0.8660254037844387076, 1.000000000000000000, 0.8660254037844387076, 1.000000000000000000, 0.8660254037844387076, 1.000000000000000000, 0.8660254037844387076, 1.000000000000000000, 0.8660254037844387076, 1.000000000000000000, 0.8660254037844387076, 1.000000000000000000, 0.8660254037844387076, 1.000000000000000000, 0.8660254037844387076, 1.000000000000000000, 0.8660254037844387076, 1.000000000000000000, 0.8660254037844387076, 1.000000000000000000, 0.8660254037844387076, 1.000000000000000000, 0.8660254037844387076, 1.000000000000000000, 0.8660254037844387076, 1.000000000000000000, 0.8660254037844387076, 1.000000000000000000, 0.8660254037844387076, 1.000000000000000000, 0.8660254037844387076, 1.000000000000000000, 0.8660254037844387076, 1.000000000000000000, 0.8660254037844387076, 1.000000000000000000, 0.8660254037844387076, 1.000000000000000000, 0.8660254037844387076, 1.000000000000000000, 0.8660254037844387076, 1.000000000000000000, 0.8660254037844387076, 1.000000000000000000, 0.8660254037844387076, 1.000000000000000000, 0.8660254037844387076, 1.000000000000000000, 0.8660254037844387076, 1.000000000000000000, 0.8660254037844387076, 1.000000000000000000, 0.8660254037844387076, 1.000000000000000000, 0.8660254037844387076, 1.000000000000000000, 0.8660254037844387076, 1.000000000000000000, 0.8660254037844387076, 1.000000000000000000, 0.8660254037844387076, 1.000000000000000000, 0.8660254037844387076, 1.000000000000000000, 0.8660254037844387076, 1.000000000000000000, 0.8660254037844387076, 1.000000000000000000, 0.8660254037844387076, 1.000000000000000000, 0.9211516195580409239, 0.9351128802560608744, 0.9351128802560608744, 0.9351128802560608744),
 ( 1.000000000000000000, 0.8660254037844387076, 1.000000000000000000, 0.8660254037844387076, 1.000000000000000000, 0.8660254037844387076, 1.000000000000000000, 0.8660254037844387076, 1.000000000000000000, 0.8660254037844387076, 1.000000000000000000, 0.8660254037844387076, 1.000000000000000000, 0.8660254037844387076, 1.000000000000000000, 0.8660254037844387076, 1.000000000000000000, 0.8660254037844387076, 1.000000000000000000, 0.8660254037844387076, 1.000000000000000000, 0.8660254037844387076, 1.000000000000000000, 0.8660254037844387076, 1.000000000000000000, 0.8660254037844387076, 1.000000000000000000, 0.8660254037844387076, 1.000000000000000000, 0.8660254037844387076, 1.000000000000000000, 0.8660254037844387076, 1.000000000000000000, 0.8660254037844387076, 1.000000000000000000, 0.8660254037844387076, 1.000000000000000000, 0.8660254037844387076, 1.000000000000000000, 0.8660254037844387076, 1.000000000000000000, 0.8660254037844387076, 1.000000000000000000, 0.8660254037844387076, 1.000000000000000000, 0.8660254037844387076, 1.000000000000000000, 0.8660254037844387076, 1.000000000000000000, 0.8660254037844387076, 1.000000000000000000, 0.8660254037844387076, 1.000000000000000000, 0.8660254037844387076, 1.000000000000000000, 0.8660254037844387076, 1.000000000000000000, 0.8660254037844387076, 1.000000000000000000, 0.8660254037844387076, 1.000000000000000000, 0.8660254037844387076, 1.000000000000000000, 0.8660254037844387076, 1.000000000000000000, 0.8660254037844387076, 1.000000000000000000, 0.8660254037844387076, 1.000000000000000000, 0.8660254037844387076, 1.000000000000000000, 0.8660254037844387076, 1.000000000000000000, 0.8660254037844387076, 1.000000000000000000, 0.8660254037844387076, 1.000000000000000000, 0.8660254037844387076, 1.000000000000000000, 0.8660254037844387076, 1.000000000000000000, 0.8660254037844387076, 1.000000000000000000, 0.8660254037844387076, 1.000000000000000000, 0.8660254037844387076, 1.000000000000000000, 0.8660254037844387076, 1.000000000000000000, 0.8660254037844387076, 1.000000000000000000, 0.8660254037844387076, 1.000000000000000000, 0.8660254037844387076, 1.000000000000000000, 0.8660254037844387076, 1.000000000000000000, 0.8660254037844387076, 1.000000000000000000, 0.8660254037844387076, 1.000000000000000000, 0.8660254037844387076, 1.000000000000000000, 0.8660254037844387076, 1.000000000000000000, 0.8660254037844387076, 1.000000000000000000, 0.8660254037844387076, 1.000000000000000000, 0.8660254037844387076, 1.000000000000000000, 0.8660254037844387076, 1.000000000000000000, 0.8660254037844387076, 1.000000000000000000, 0.8660254037844387076, 1.000000000000000000, 0.8660254037844387076, 1.000000000000000000, 0.8660254037844387076, 1.000000000000000000, 0.8660254037844387076, 1.000000000000000000, 0.8660254037844387076, 1.000000000000000000, 0.8660254037844387076, 1.000000000000000000, 0.8660254037844387076, 1.000000000000000000, 0.8660254037844387076, 1.000000000000000000, 0.8660254037844387076, 1.000000000000000000, 0.8660254037844387076, 1.000000000000000000, 0.8660254037844387076, 1.000000000000000000, 0.8660254037844387076, 1.000000000000000000, 0.8660254037844387076, 1.000000000000000000, 0.8660254037844387076, 1.000000000000000000, 0.8660254037844387076, 1.000000000000000000, 0.8660254037844387076, 1.000000000000000000, 0.8660254037844387076, 1.000000000000000000, 0.8660254037844387076, 1.000000000000000000, 0.9211516195580409239, 0.9351128802560608744, 0.9351128802560608744, 0.9351128802560608744) ) ) 
 REPRESENTATION_ITEM ( '' )  SURFACE ( )  );
#298 = CARTESIAN_POINT ( 'NONE',  ( 26.51200394741821498, -4.842675973971495296, -7.939653947423662039 ) ) ;
#299 = ADVANCED_FACE ( 'NONE', ( #4183 ), #15505, .F. ) ;
#300 = ORIENTED_EDGE ( 'NONE', *, *, #10123, .T. ) ;
#301 = CARTESIAN_POINT ( 'NONE',  ( 30.45225960443380231, -4.367952981209816343, -3.627061608673664672 ) ) ;
#302 = CARTESIAN_POINT ( 'NONE',  ( -0.6507732100473456738, 4.243078065514776398, -0.2236248678334832318 ) ) ;
#303 = CARTESIAN_POINT ( 'NONE',  ( 30.08145424927873535, -6.930706697444451336, 5.783357778048664244 ) ) ;
#304 = DIRECTION ( 'NONE',  ( 1.000000000000000000, 0.000000000000000000, 0.000000000000000000 ) ) ;
#305 = CARTESIAN_POINT ( 'NONE',  ( 33.16732689266149237, -6.221561368663743430, -7.033357778048666908 ) ) ;
#306 = DIRECTION ( 'NONE',  ( 0.6000000000000000888, 0.7999999999999999334, 0.000000000000000000 ) ) ;
#307 = EDGE_CURVE ( 'NONE', #987, #12566, #1185, .T. ) ;
#308 = ORIENTED_EDGE ( 'NONE', *, *, #12713, .F. ) ;
#309 = CARTESIAN_POINT ( 'NONE',  ( 33.14902674121363901, -1.535163666906202318, 5.783357778048668685 ) ) ;
#310 = AXIS2_PLACEMENT_3D ( 'NONE', #17045, #11193, #5866 ) ;
#311 = B_SPLINE_CURVE_WITH_KNOTS ( 'NONE', 3,
 ( #3913, #14963, #2548, #9253, #15054, #13611, #2295, #12250, #7815, #6459, #11975, #3828, #10680, #14798, #10859, #16254 ),
 .UNSPECIFIED., .F., .F.,
 ( 4, 2, 2, 2, 2, 2, 2, 4 ),
 ( 0.000000000000000000, 0.0008414457502979328513, 0.001262168625446899277, 0.001682891500595865703, 0.002103614375744832128, 0.002524337250893798554, 0.002945060126042764979, 0.003365783001191731405 ),
 .UNSPECIFIED. ) ;
#312 = CLOSED_SHELL ( 'NONE', ( #13052, #4033, #17691, #12015, #10916, #12800, #4306, #10100, #2178, #4714, #3417, #147, #13494, #15586, #15060, #10969, #7511, #8648, #5633, #10348, #2026, #9611, #12090, #6179, #12893, #7460, #15673 ) ) ;
#313 = PRESENTATION_LAYER_ASSIGNMENT (  '', '', ( #15961 ) ) ;
#314 = CARTESIAN_POINT ( 'NONE',  ( 27.45766530510195835, -4.728742455708699666, 7.939653947423662039 ) ) ;
#315 = CARTESIAN_POINT ( 'NONE',  ( -25.01192583800304448, -22.13892749297381002, 14.47384481777684151 ) ) ;
#316 = CARTESIAN_POINT ( 'NONE',  ( 0.000000000000000000, 0.000000000000000000, -4.000000000000000000 ) ) ;
#317 = VERTEX_POINT ( 'NONE', #12603 ) ;
#318 = ORIENTED_EDGE ( 'NONE', *, *, #17763, .T. ) ;
#319 = DIRECTION ( 'NONE',  ( -0.000000000000000000, 1.000000000000000000, 0.000000000000000000 ) ) ;
#320 =( BOUNDED_CURVE ( )  B_SPLINE_CURVE ( 2, ( #15229, #5785, #179, #16687, #11299, #4179, #6980, #13960, #12681 ),
 .UNSPECIFIED., .F., .T. ) 
 B_SPLINE_CURVE_WITH_KNOTS ( ( 3, 2, 2, 2, 3 ),
 ( 0.5192307692307692735, 0.5256410256410256610, 0.5384615384615384359, 0.5512820512820513219, 0.5576923076923077094 ),
 .UNSPECIFIED. ) 
 CURVE ( )  GEOMETRIC_REPRESENTATION_ITEM ( )  RATIONAL_B_SPLINE_CURVE ( ( 0.9330127018922192983, 0.9330127018922198534, 1.000000000000000000, 0.8660254037844387076, 1.000000000000000000, 0.8660254037844387076, 1.000000000000000000, 0.9330127018922194093, 0.9330127018922194093 ) ) 
 REPRESENTATION_ITEM ( '' )  );
#321 = ORIENTED_EDGE ( 'NONE', *, *, #9994, .T. ) ;
#322 = ORIENTED_EDGE ( 'NONE', *, *, #10221, .F. ) ;
#323 = CARTESIAN_POINT ( 'NONE',  ( 30.17644170758179101, -4.401183590806859947, -3.283357778048664688 ) ) ;
#324 = CIRCLE ( 'NONE', #13067, 2.000000000000001776 ) ;
#325 = CARTESIAN_POINT ( 'NONE',  ( 27.28266178881210280, -7.257709054644824853, -5.783357778048669573 ) ) ;
#326 = ADVANCED_FACE ( 'NONE', ( #3086 ), #2732, .F. ) ;
#327 = CARTESIAN_POINT ( 'NONE',  ( 31.11087420047036289, -5.742416513891037688, -3.283357778048667797 ) ) ;
#328 = DIRECTION ( 'NONE',  ( 1.000000000000000000, 0.000000000000000000, 0.000000000000000000 ) ) ;
#329 = FACE_BOUND ( 'NONE', #8817, .T. ) ;
#330 =( REPRESENTATION_RELATIONSHIP ('NONE','NONE', #3227, #1480 ) REPRESENTATION_RELATIONSHIP_WITH_TRANSFORMATION ( #17298 )SHAPE_REPRESENTATION_RELATIONSHIP( ) );
#331 = CARTESIAN_POINT ( 'NONE',  ( 29.04699097144805364, -6.418171698071525100, -4.705209693361169343 ) ) ;
#332 = CARTESIAN_POINT ( 'NONE',  ( 32.17274868998081416, -2.279756424927169345, -4.705209693361160461 ) ) ;
#333 = DIRECTION ( 'NONE',  ( 1.000000000000000000, 0.000000000000000000, -0.000000000000000000 ) ) ;
#334 = DIRECTION ( 'NONE',  ( 0.9928203230275510771, 0.1196152422706614205, 0.000000000000000000 ) ) ;
#335 = EDGE_CURVE ( 'NONE', #2070, #225, #4373, .T. ) ;
#336 = CARTESIAN_POINT ( 'NONE',  ( 32.07220196432897552, -5.426722983814484813, 7.939653947423658487 ) ) ;
#337 = ORIENTED_EDGE ( 'NONE', *, *, #15957, .T. ) ;
#338 = VECTOR ( 'NONE', #16087, 1000.000000000000000 ) ;
#339 = ORIENTED_EDGE ( 'NONE', *, *, #15948, .F. ) ;
#340 = EDGE_CURVE ( 'NONE', #8339, #14403, #8608, .T. ) ;
#341 = CARTESIAN_POINT ( 'NONE',  ( 27.61527553138257574, -4.709753535998224550, 3.627061608673664228 ) ) ;
#342 = CARTESIAN_POINT ( 'NONE',  ( -45.00000000000000711, -19.03270077640483038, 5.537981825772250843 ) ) ;
#343 = CARTESIAN_POINT ( 'NONE',  ( -36.27615609941022257, -23.17738945083361557, 0.000000000000000000 ) ) ;
#344 = ORIENTED_EDGE ( 'NONE', *, *, #4632, .T. ) ;
#345 = FILL_AREA_STYLE ('',( #12748 ) ) ;
#346 = ORIENTED_EDGE ( 'NONE', *, *, #15420, .F. ) ;
#347 = DIRECTION ( 'NONE',  ( 0.000000000000000000, 0.5027044994213121232, -0.8644583195629318428 ) ) ;
#348 = CARTESIAN_POINT ( 'NONE',  ( 31.80137159822941939, -6.386132006154467078, -4.533357778048668685 ) ) ;
#349 = CARTESIAN_POINT ( 'NONE',  ( 33.56434302664245450, -9.029166375164061620, -5.783357778048662468 ) ) ;
#350 = FACE_OUTER_BOUND ( 'NONE', #12268, .T. ) ;
#351 = ORIENTED_EDGE ( 'NONE', *, *, #12885, .F. ) ;
#352 = CARTESIAN_POINT ( 'NONE',  ( 27.36943512155133362, -2.558652073080304845, -4.533357778048659803 ) ) ;
#353 = CARTESIAN_POINT ( 'NONE',  ( -23.00000000000000000, -16.21813761408365195, -13.00000000000000178 ) ) ;
#354 = AXIS2_PLACEMENT_3D ( 'NONE', #5840, #1963, #15742 ) ;
#355 = CARTESIAN_POINT ( 'NONE',  ( -20.00000000000000000, 7.999999999999996447, 12.00000000000000000 ) ) ;
#356 = CARTESIAN_POINT ( 'NONE',  ( 30.02326902268086428, -5.673578940050561847, -3.627061608673667781 ) ) ;
#357 = AXIS2_PLACEMENT_3D ( 'NONE', #9695, #13538, #6726 ) ;
#358 = CYLINDRICAL_SURFACE ( 'NONE', #310, 5.000000000000000000 ) ;
#359 = CARTESIAN_POINT ( 'NONE',  ( 0.000000000000000000, 0.000000000000000000, -2.000000000000000000 ) ) ;
#360 = AXIS2_PLACEMENT_3D ( 'NONE', #8254, #1099, #13788 ) ;
#361 = ORIENTED_EDGE ( 'NONE', *, *, #14655, .T. ) ;
#362 = ORIENTED_EDGE ( 'NONE', *, *, #13450, .F. ) ;
#363 = ORIENTED_EDGE ( 'NONE', *, *, #1585, .T. ) ;
#364 = VERTEX_POINT ( 'NONE', #16969 ) ;
#365 = ADVANCED_FACE ( 'NONE', ( #4, #13869 ), #9593, .F. ) ;
#366 = CARTESIAN_POINT ( 'NONE',  ( 29.99682221560115991, -1.914942061115552541, 5.783357778048668685 ) ) ;
#367 = AXIS2_PLACEMENT_3D ( 'NONE', #11007, #6593, #15201 ) ;
#368 = DIRECTION ( 'NONE',  ( -0.1196152422706609625, 0.9928203230275510771, 0.000000000000000000 ) ) ;
#369 = DIRECTION ( 'NONE',  ( 0.000000000000000000, 0.000000000000000000, 1.000000000000000000 ) ) ;
#370 = DIRECTION ( 'NONE',  ( -0.7999999999999999334, -0.6000000000000001998, 0.000000000000000000 ) ) ;
#371 = LINE ( 'NONE', #5878, #16268 ) ;
#372 = CARTESIAN_POINT ( 'NONE',  ( 32.91278983782564183, -5.325448745358647429, -7.939653947423664704 ) ) ;
#373 = CARTESIAN_POINT ( 'NONE',  ( 30.05329989404488700, -6.934098741245490416, -5.113484796970860558 ) ) ;
#374 = DIRECTION ( 'NONE',  ( 0.9928203230275512992, 0.1196152422706610180, 4.006172263299093133E-17 ) ) ;
#375 = CIRCLE ( 'NONE', #6145, 13.00000000000000178 ) ;
#376 = AXIS2_PLACEMENT_3D ( 'NONE', #11104, #8407, #9745 ) ;
#377 = DIRECTION ( 'NONE',  ( -0.6174492339697512655, -0.7866107318554506067, 0.000000000000000000 ) ) ;
#378 = EDGE_CURVE ( 'NONE', #2087, #11687, #3800, .T. ) ;
#379 = CARTESIAN_POINT ( 'NONE',  ( 27.82847066025702887, -2.165988739474055791, -5.783357778048658027 ) ) ;
#380 = CARTESIAN_POINT ( 'NONE',  ( 29.62036837594175154, -3.214238380052812261, -3.627061608673662896 ) ) ;
#381 = CARTESIAN_POINT ( 'NONE',  ( -2.016448651773435938E-27, -20.49999999999999645, 13.00000000000000178 ) ) ;
#382 = DIRECTION ( 'NONE',  ( -0.000000000000000000, -0.000000000000000000, 1.000000000000000000 ) ) ;
#383 = CARTESIAN_POINT ( 'NONE',  ( 25.97837335112617652, -4.585712065882579402, -3.626324104489874411 ) ) ;
#384 = CARTESIAN_POINT ( 'NONE',  ( 28.05993251931039012, -3.202367565343740452, 8.283357778048666020 ) ) ;
#385 = CARTESIAN_POINT ( 'NONE',  ( 29.81239362717914787, -2.264323817775507397, 7.033357778048666020 ) ) ;
#386 = FACE_OUTER_BOUND ( 'NONE', #5358, .T. ) ;
#387 = ORIENTED_EDGE ( 'NONE', *, *, #378, .F. ) ;
#388 = ADVANCED_FACE ( 'NONE', ( #5520 ), #11038, .F. ) ;
#389 = ADVANCED_FACE ( 'NONE', ( #12512 ), #15232, .T. ) ;
#390 = DIRECTION ( 'NONE',  ( 0.9928203230275510771, 0.1196152422706609902, 4.006172263299092517E-17 ) ) ;
#391 = DIRECTION ( 'NONE',  ( 0.000000000000000000, 0.000000000000000000, 1.000000000000000000 ) ) ;
#392 = ORIENTED_EDGE ( 'NONE', *, *, #2514, .T. ) ;
#393 = CYLINDRICAL_SURFACE ( 'NONE', #607, 6.249999999999998224 ) ;
#394 = VECTOR ( 'NONE', #8237, 1000.000000000000114 ) ;
#395 = ORIENTED_EDGE ( 'NONE', *, *, #4966, .T. ) ;
#396 = CARTESIAN_POINT ( 'NONE',  ( 28.54354359905709160, -7.105797696961086096, -5.783357778048669573 ) ) ;
#397 = VERTEX_POINT ( 'NONE', #1454 ) ;
#398 = CARTESIAN_POINT ( 'NONE',  ( 31.25770402584614516, -1.763030703431812674, -5.783357778048658027 ) ) ;
#399 = CARTESIAN_POINT ( 'NONE',  ( 33.95908713831674675, -3.945449517755636126, -5.783357778048663356 ) ) ;
#400 = CARTESIAN_POINT ( 'NONE',  ( 25.71748644841968456, -2.420320648352051851, -5.783357778048663356 ) ) ;
#401 = DIRECTION ( 'NONE',  ( 0.000000000000000000, 0.000000000000000000, -1.000000000000000000 ) ) ;
#402 = ORIENTED_EDGE ( 'NONE', *, *, #10796, .T. ) ;
#403 = CARTESIAN_POINT ( 'NONE',  ( 31.59864285835955400, -2.049116061056871274, -7.033357778048658027 ) ) ;
#404 = DIRECTION ( 'NONE',  ( -0.6000000000000000888, -0.7999999999999999334, 0.000000000000000000 ) ) ;
#405 = ORIENTED_EDGE ( 'NONE', *, *, #3183, .F. ) ;
#406 = CARTESIAN_POINT ( 'NONE',  ( 25.52694003402523748, -4.961356722058193114, 3.283357778048664244 ) ) ;
#407 =( BOUNDED_CURVE ( )  B_SPLINE_CURVE ( 3, ( #13282, #6744, #6491, #3856 ),
 .UNSPECIFIED., .F., .T. ) 
 B_SPLINE_CURVE_WITH_KNOTS ( ( 4, 4 ),
 ( 1.825438360997748255, 1.919862177193756514 ),
 .UNSPECIFIED. ) 
 CURVE ( )  GEOMETRIC_REPRESENTATION_ITEM ( )  RATIONAL_B_SPLINE_CURVE ( ( 1.000000000000000000, 0.9992571499088201969, 0.9992571499088201969, 1.000000000000000000 ) ) 
 REPRESENTATION_ITEM ( '' )  );
#408 = EDGE_CURVE ( 'NONE', #7873, #17484, #97, .T. ) ;
#409 = CARTESIAN_POINT ( 'NONE',  ( -8.249999999999923617, 6.495190528383386841, -3.000000000000002665 ) ) ;
#410 = CARTESIAN_POINT ( 'NONE',  ( -16.75000000000000000, -16.21813761408365195, 16.03574476417183448 ) ) ;
#411 = CARTESIAN_POINT ( 'NONE',  ( 25.71748644841968456, -2.420320648352051851, -5.783357778048663356 ) ) ;
#412 = EDGE_LOOP ( 'NONE', ( #5824, #3661, #12344, #1418, #13778, #8078, #11628, #2736, #4071, #7877, #15831 ) ) ;
#413 = CARTESIAN_POINT ( 'NONE',  ( 26.18940075748478691, -6.337263906362392341, 3.743184633113769699 ) ) ;
#414 = ORIENTED_EDGE ( 'NONE', *, *, #10725, .T. ) ;
#415 = CARTESIAN_POINT ( 'NONE',  ( -10.50000000000000000, -1.591841644184202181E-21, -6.005572809000082835 ) ) ;
#416 = CARTESIAN_POINT ( 'NONE',  ( 25.96530230012339757, -2.390463732198628399, -5.113484796970851676 ) ) ;
#417 = ORIENTED_EDGE ( 'NONE', *, *, #1398, .F. ) ;
#418 = CARTESIAN_POINT ( 'NONE',  ( 0.000000000000000000, 0.000000000000000000, 13.31572692736085095 ) ) ;
#419 = EDGE_CURVE ( 'NONE', #15092, #4502, #11122, .T. ) ;
#420 = CARTESIAN_POINT ( 'NONE',  ( 25.76326615456878244, -3.051972493152843580, -6.861505862736158257 ) ) ;
#421 = CARTESIAN_POINT ( 'NONE',  ( 30.38277803966508372, -1.468696967828331701, -5.783357778048658027 ) ) ;
#422 = CARTESIAN_POINT ( 'NONE',  ( -9.099998387031003944, -19.29508120620799616, 12.00000000000000000 ) ) ;
#423 = CARTESIAN_POINT ( 'NONE',  ( 33.81344892038539740, -6.481075040654873831, 5.113484796970855228 ) ) ;
#424 = CARTESIAN_POINT ( 'NONE',  ( 29.76058531221316628, -5.705227139567997874, -7.939653947423664704 ) ) ;
#425 = CARTESIAN_POINT ( 'NONE',  ( 32.95080301609915097, -1.548848848676412260, -5.783357778048662468 ) ) ;
#426 = CARTESIAN_POINT ( 'NONE',  ( 8.632250723006720250, -18.84644399697197770, 16.84735068286506987 ) ) ;
#427 = CARTESIAN_POINT ( 'NONE',  ( -8.874038404635992805, -3.391377654146690013, -2.000000000000000000 ) ) ;
#428 = CARTESIAN_POINT ( 'NONE',  ( 30.19827253897071273, -3.144612341114420673, 3.627061608673666893 ) ) ;
#429 = ORIENTED_EDGE ( 'NONE', *, *, #16185, .F. ) ;
#430 = CARTESIAN_POINT ( 'NONE',  ( 26.97161122272022382, -2.906390775372597712, -4.705209693361161349 ) ) ;
#431 = EDGE_CURVE ( 'NONE', #3807, #1473, #11303, .T. ) ;
#432 =( BOUNDED_CURVE ( )  B_SPLINE_CURVE ( 2, ( #7895, #3983, #3719, #2460, #1275, #16246, #6699, #3817, #13689 ),
 .UNSPECIFIED., .F., .T. ) 
 B_SPLINE_CURVE_WITH_KNOTS ( ( 3, 2, 2, 2, 3 ),
 ( 0.2115384615384615641, 0.2179487179487179516, 0.2307692307692307820, 0.2435897435897435848, 0.2500000000000000000 ),
 .UNSPECIFIED. ) 
 CURVE ( )  GEOMETRIC_REPRESENTATION_ITEM ( )  RATIONAL_B_SPLINE_CURVE ( ( 0.9330127018922194093, 0.9330127018922196314, 1.000000000000000000, 0.8660254037844387076, 1.000000000000000000, 0.8660254037844387076, 1.000000000000000000, 0.9330127018922191873, 0.9330127018922194093 ) ) 
 REPRESENTATION_ITEM ( '' )  );
#433 = ORIENTED_EDGE ( 'NONE', *, *, #8405, .T. ) ;
#434 = CARTESIAN_POINT ( 'NONE',  ( 28.36401332423200827, -6.500457016816879374, 4.705209693361160461 ) ) ;
#435 = CARTESIAN_POINT ( 'NONE',  ( 32.14656953781143756, -4.163822094218565972, -3.283357778048664688 ) ) ;
#436 = CARTESIAN_POINT ( 'NONE',  ( 25.98779870451785001, -2.387753359738024272, -6.453230759126469707 ) ) ;
#437 = ORIENTED_EDGE ( 'NONE', *, *, #17620, .F. ) ;
#438 = CARTESIAN_POINT ( 'NONE',  ( 28.51030546511822195, -6.055733689321201041, -3.283357778048667797 ) ) ;
#439 = EDGE_LOOP ( 'NONE', ( #6272, #4236, #9102, #14227 ) ) ;
#440 = FACE_OUTER_BOUND ( 'NONE', #9087, .T. ) ;
#441 = ORIENTED_EDGE ( 'NONE', *, *, #16657, .T. ) ;
#442 = DIRECTION ( 'NONE',  ( 1.000000000000000000, 0.000000000000000000, 0.000000000000000000 ) ) ;
#443 = EDGE_CURVE ( 'NONE', #1609, #16681, #2190, .T. ) ;
#444 = ADVANCED_FACE ( 'NONE', ( #17342 ), #8707, .T. ) ;
#445 = CARTESIAN_POINT ( 'NONE',  ( 26.20620856698912604, -7.060238655668615415, -4.533357778048668685 ) ) ;
#446 = CARTESIAN_POINT ( 'NONE',  ( -8.632250723006720250, -18.84644399697197770, 13.00000000000000178 ) ) ;
#447 = SHAPE_REPRESENTATION_RELATIONSHIP ( 'NONE' , 'NONE' ,  #12009, #11756 ) ;
#448 = CARTESIAN_POINT ( 'NONE',  ( 32.14213199643172914, -2.910415664685331638, -3.627061608673662896 ) ) ;
#449 = EDGE_LOOP ( 'NONE', ( #10237, #6974, #15692, #17847 ) ) ;
#450 = CARTESIAN_POINT ( 'NONE',  ( 26.16909369068367752, -6.168712907020689862, -7.925803108758818105 ) ) ;
#451 = CARTESIAN_POINT ( 'NONE',  ( 30.48043329534786849, -5.818372192732907067, 8.283357778048658915 ) ) ;
#452 = ORIENTED_EDGE ( 'NONE', *, *, #3011, .F. ) ;
#453 = ORIENTED_EDGE ( 'NONE', *, *, #654, .T. ) ;
#454 = ORIENTED_EDGE ( 'NONE', *, *, #8512, .T. ) ;
#455 = CARTESIAN_POINT ( 'NONE',  ( 30.13703915187255689, -4.405930820630744371, 3.627061608673664228 ) ) ;
#456 = CARTESIAN_POINT ( 'NONE',  ( 26.45077056032005913, -6.103994453487816330, -7.939653947423662927 ) ) ;
#457 = CARTESIAN_POINT ( 'NONE',  ( 0.000000000000000000, 0.000000000000000000, 8.700000000000001066 ) ) ;
#458 = FACE_BOUND ( 'NONE', #16476, .T. ) ;
#459 = CARTESIAN_POINT ( 'NONE',  ( -15.92260893619738837, -28.39189527176317540, 16.15082599432113142 ) ) ;
#460 = CARTESIAN_POINT ( 'NONE',  ( 31.43723430067123914, -2.368371383576012956, -6.861505862736158257 ) ) ;
#461 = LINE ( 'NONE', #1551, #9865 ) ;
#462 = LINE ( 'NONE', #8801, #7562 ) ;
#463 = LINE ( 'NONE', #8609, #11325 ) ;
#464 = FACE_OUTER_BOUND ( 'NONE', #9098, .T. ) ;
#465 = ADVANCED_FACE ( 'NONE', ( #10138 ), #11491, .T. ) ;
#466 = CARTESIAN_POINT ( 'NONE',  ( 33.56515079149260572, -5.873822666371450119, -6.861505862736167138 ) ) ;
#467 = CARTESIAN_POINT ( 'NONE',  ( -5.781152949374543937, -1.605699403978851247, -2.000000000000000000 ) ) ;
#468 = DIRECTION ( 'NONE',  ( -1.000000000000000000, 0.000000000000000000, 0.000000000000000000 ) ) ;
#469 = CARTESIAN_POINT ( 'NONE',  ( 4.207491450040567571, -2.029819825146481183, -3.371670828759568028 ) ) ;
#470 = PLANE ( 'NONE',  #13831 ) ;
#471 = CARTESIAN_POINT ( 'NONE',  ( 27.78220930431293922, -1.782014143258494832, 5.783357778048668685 ) ) ;
#472 = CARTESIAN_POINT ( 'NONE',  ( 26.66961417369883591, -4.823687054261037055, -3.627061608673664672 ) ) ;
#473 = EDGE_LOOP ( 'NONE', ( #2498, #12388, #7781 ) ) ;
#474 = CARTESIAN_POINT ( 'NONE',  ( -45.00000000000000711, -19.03270077640483038, -5.537981825772250843 ) ) ;
#475 = VERTEX_POINT ( 'NONE', #2002 ) ;
#476 = CARTESIAN_POINT ( 'NONE',  ( 29.08935247050201767, -2.014077381790315702, -5.783357778048658027 ) ) ;
#477 = DIRECTION ( 'NONE',  ( -0.000000000000000000, -0.000000000000000000, 1.000000000000000000 ) ) ;
#478 = DIRECTION ( 'NONE',  ( -0.9928203230275512992, -0.1196152422706610180, -4.006172263299093133E-17 ) ) ;
#479 = CARTESIAN_POINT ( 'NONE',  ( 25.86833963875586306, -3.039313213345869791, -4.705209693361160461 ) ) ;
#480 = EDGE_CURVE ( 'NONE', #2781, #625, #723, .T. ) ;
#481 = CARTESIAN_POINT ( 'NONE',  ( 30.88125018618674744, -3.062327022369072171, -3.627061608673662896 ) ) ;
#482 = ORIENTED_EDGE ( 'NONE', *, *, #16676, .F. ) ;
#483 = CARTESIAN_POINT ( 'NONE',  ( 3.035766082959412415E-15, 4.618802153517010289, -0.5000000000000000000 ) ) ;
#484 = CARTESIAN_POINT ( 'NONE',  ( 29.37220822929407760, -7.016156836349003001, -5.783357778048668685 ) ) ;
#485 = CARTESIAN_POINT ( 'NONE',  ( 27.21934464581372737, -3.303641803799556964, 3.283357778048666464 ) ) ;
#486 = CARTESIAN_POINT ( 'NONE',  ( 30.64556327217151122, -6.525384084031224496, -7.033357778048666908 ) ) ;
#487 = CARTESIAN_POINT ( 'NONE',  ( -23.00000000000000000, -16.21813761408365195, 0.000000000000000000 ) ) ;
#488 = CARTESIAN_POINT ( 'NONE',  ( 26.34507017448785504, -7.770415366711231009, 5.783357778048657138 ) ) ;
#489 = PLANE ( 'NONE',  #1672 ) ;
#490 = DIRECTION ( 'NONE',  ( 0.9928203230275512992, 0.1196152422706614482, 0.000000000000000000 ) ) ;
#491 = ORIENTED_EDGE ( 'NONE', *, *, #2769, .T. ) ;
#492 = FACE_OUTER_BOUND ( 'NONE', #1631, .T. ) ;
#493 = ORIENTED_EDGE ( 'NONE', *, *, #7842, .T. ) ;
#494 = DIRECTION ( 'NONE',  ( 0.9928203230275510771, 0.1196152422706609902, 4.006172263299092517E-17 ) ) ;
#495 = CARTESIAN_POINT ( 'NONE',  ( -36.27615609941022257, -23.17738945083361557, 0.000000000000000000 ) ) ;
#496 = VERTEX_POINT ( 'NONE', #3169 ) ;
#497 = DIRECTION ( 'NONE',  ( 0.000000000000000000, 0.000000000000000000, 1.000000000000000000 ) ) ;
#498 = ADVANCED_FACE ( 'NONE', ( #4791 ), #9064, .T. ) ;
#499 = CYLINDRICAL_SURFACE ( 'NONE', #17938, 2.500000000000001776 ) ;
#500 = CARTESIAN_POINT ( 'NONE',  ( 0.000000000000000000, 0.000000000000000000, 0.000000000000000000 ) ) ;
#501 = EDGE_CURVE ( 'NONE', #82, #692, #8780, .T. ) ;
#502 = CYLINDRICAL_SURFACE ( 'NONE', #6351, 5.500000000000000888 ) ;
#503 = CARTESIAN_POINT ( 'NONE',  ( 32.93470988637010066, -5.949778345213319497, -6.861505862736167138 ) ) ;
#504 = DIRECTION ( 'NONE',  ( 1.000000000000000000, 0.000000000000000000, 0.000000000000000000 ) ) ;
#505 = DIRECTION ( 'NONE',  ( 0.7999999999999999334, -0.6000000000000001998, 0.000000000000000000 ) ) ;
#506 = CARTESIAN_POINT ( 'NONE',  ( 30.41294626588012306, -6.253601060580800564, 4.705209693361159573 ) ) ;
#507 =( BOUNDED_CURVE ( )  B_SPLINE_CURVE ( 2, ( #5175, #2560, #10530, #5264, #17744, #16361, #6371, #3573, #10783, #16267, #2398, #10692, #11894, #3839, #3923, #14892, #17569, #16091, #9353, #8087, #9435, #1029, #2477, #3658, #6550, #13259, #14975, #2219, #753, #6472, #7999, #9265, #14724, #16177, #9179, #12067, #4913, #2307, #6279, #10440, #13356, #13535, #1109, #6634, #11800, #17378, #5089, #7825, #9096, #11986, #16000, #17474, #3740, #936, #14638, #10610, #841, #14809, #7914, #13448, #17652, #8181, #1205, #9778, #9873, #12614, #11052, #16614, #8263, #16439, #2909, #8348, #11220, #16, #4096, #9692, #16795, #1563, #2652, #4007, #4363, #12261, #6818, #9520, #5348, #15428, #3013, #11132, #15066, #12428, #10959, #5705, #13623, #13714, #12343, #1295, #2820, #6721, #17910, #6995, #17829, #5441, #5615, #15331, #2743, #10869, #13880, #16520, #9604, #15160, #193, #16701, #13795, #1376, #6901, #5529, #4275, #8441, #4190, #15240, #13977, #1467, #12523, #109, #7096, #7371, #5978, #5800, #14253, #11503, #4627, #11316, #472, #14069, #12790, #4536, #17074, #11415, #289, #15701, #16896, #10151, #5894, #7187, #15516, #4455, #10056 ),
 .UNSPECIFIED., .F., .T. ) 
 B_SPLINE_CURVE_WITH_KNOTS ( ( 3, 2, 2, 2, 2, 2, 2, 2, 2, 2, 2, 2, 2, 2, 2, 2, 2, 2, 2, 2, 2, 2, 2, 2, 2, 2, 2, 2, 2, 2, 2, 2, 2, 2, 2, 2, 2, 2, 2, 2, 2, 2, 2, 2, 2, 2, 2, 2, 2, 2, 2, 2, 2, 2, 2, 2, 2, 2, 2, 2, 2, 2, 2, 2, 2, 2, 2, 2, 2, 2, 2, 2, 2, 3 ),
 ( 0.000000000000000000, 0.01322951968774666726, 0.02645903937549333451, 0.03968855906324000177, 0.05291807875098666902, 0.06614759843873332934, 0.07937711812648000353, 0.09260663781422667773, 0.1058361575019733380, 0.1190656771897200122, 0.1322951968774666587, 0.1455247165652133190, 0.1587542362529600071, 0.1719837559407066396, 0.1852132756284533555, 0.1984427953162000158, 0.2116723150039466761, 0.2249018346916933364, 0.2381313543794400245, 0.2513608740671866570, 0.2645903937549333174, 0.2778199134426800332, 0.2910494331304266380, 0.3042789528181733538, 0.3175084725059200141, 0.3307379921936667300, 0.3439675118814132793, 0.3571970315691599951, 0.3704265512569067109, 0.3836560709446533712, 0.3968855906324000316, 0.4101151103201466364, 0.4233446300078933522, 0.4365741496956400125, 0.4498036693833866728, 0.4630331890711333331, 0.4762627087588800490, 0.4894922284466267093, 0.5027217481343733141, 0.5159512678221199744, 0.5291807875098666347, 0.5424103071976132950, 0.5556398268853600664, 0.5688693465731067267, 0.5820988662608532760, 0.5953283859485999363, 0.6085579056363467076, 0.6217874253240932569, 0.6350169450118400283, 0.6482464646995866886, 0.6614759843873334599, 0.6747055040750800092, 0.6879350237628265585, 0.7011645434505734409, 0.7143940631383199902, 0.7276235828260666505, 0.7408531025138134218, 0.7540826222015599711, 0.7673121418893067425, 0.7805416615770532918, 0.7937711812648000631, 0.8070007009525467234, 0.8202302206402932727, 0.8334597403280399330, 0.8466892600157867044, 0.8599187797035333647, 0.8731482993912800250, 0.8863778190790266853, 0.8996073387667733456, 0.9128368584545200060, 0.9260663781422666663, 0.9392958978300133266, 0.9525254175177600979, 0.9555550897579921932 ),
 .UNSPECIFIED. ) 
 CURVE ( )  GEOMETRIC_REPRESENTATION_ITEM ( )  RATIONAL_B_SPLINE_CURVE ( ( 1.000000000000000000, 0.8660254037844387076, 1.000000000000000000, 0.8660254037844387076, 1.000000000000000000, 0.8660254037844387076, 1.000000000000000000, 0.8660254037844387076, 1.000000000000000000, 0.8660254037844387076, 1.000000000000000000, 0.8660254037844387076, 1.000000000000000000, 0.8660254037844387076, 1.000000000000000000, 0.8660254037844387076, 1.000000000000000000, 0.8660254037844387076, 1.000000000000000000, 0.8660254037844387076, 1.000000000000000000, 0.8660254037844387076, 1.000000000000000000, 0.8660254037844387076, 1.000000000000000000, 0.8660254037844387076, 1.000000000000000000, 0.8660254037844387076, 1.000000000000000000, 0.8660254037844387076, 1.000000000000000000, 0.8660254037844387076, 1.000000000000000000, 0.8660254037844387076, 1.000000000000000000, 0.8660254037844387076, 1.000000000000000000, 0.8660254037844387076, 1.000000000000000000, 0.8660254037844387076, 1.000000000000000000, 0.8660254037844387076, 1.000000000000000000, 0.8660254037844387076, 1.000000000000000000, 0.8660254037844387076, 1.000000000000000000, 0.8660254037844387076, 1.000000000000000000, 0.8660254037844387076, 1.000000000000000000, 0.8660254037844387076, 1.000000000000000000, 0.8660254037844387076, 1.000000000000000000, 0.8660254037844387076, 1.000000000000000000, 0.8660254037844387076, 1.000000000000000000, 0.8660254037844387076, 1.000000000000000000, 0.8660254037844387076, 1.000000000000000000, 0.8660254037844387076, 1.000000000000000000, 0.8660254037844387076, 1.000000000000000000, 0.8660254037844387076, 1.000000000000000000, 0.8660254037844387076, 1.000000000000000000, 0.8660254037844387076, 1.000000000000000000, 0.8660254037844387076, 1.000000000000000000, 0.8660254037844387076, 1.000000000000000000, 0.8660254037844387076, 1.000000000000000000, 0.8660254037844387076, 1.000000000000000000, 0.8660254037844387076, 1.000000000000000000, 0.8660254037844387076, 1.000000000000000000, 0.8660254037844387076, 1.000000000000000000, 0.8660254037844387076, 1.000000000000000000, 0.8660254037844387076, 1.000000000000000000, 0.8660254037844387076, 1.000000000000000000, 0.8660254037844387076, 1.000000000000000000, 0.8660254037844387076, 1.000000000000000000, 0.8660254037844387076, 1.000000000000000000, 0.8660254037844387076, 1.000000000000000000, 0.8660254037844387076, 1.000000000000000000, 0.8660254037844387076, 1.000000000000000000, 0.8660254037844387076, 1.000000000000000000, 0.8660254037844387076, 1.000000000000000000, 0.8660254037844387076, 1.000000000000000000, 0.8660254037844387076, 1.000000000000000000, 0.8660254037844387076, 1.000000000000000000, 0.8660254037844387076, 1.000000000000000000, 0.8660254037844387076, 1.000000000000000000, 0.8660254037844387076, 1.000000000000000000, 0.8660254037844387076, 1.000000000000000000, 0.8660254037844387076, 1.000000000000000000, 0.8660254037844387076, 1.000000000000000000, 0.8660254037844387076, 1.000000000000000000, 0.8660254037844387076, 1.000000000000000000, 0.8660254037844387076, 1.000000000000000000, 0.8660254037844387076, 1.000000000000000000, 0.8660254037844387076, 1.000000000000000000, 0.8660254037844387076, 1.000000000000000000, 0.8660254037844387076, 1.000000000000000000, 0.8660254037844387076, 1.000000000000000000, 0.8660254037844387076, 1.000000000000000000, 0.9693186809021840933, 0.9526899265169710418 ) ) 
 REPRESENTATION_ITEM ( '' )  );
#508 = AXIS2_PLACEMENT_3D ( 'NONE', #1126, #17848, #9453 ) ;
#509 = ORIENTED_EDGE ( 'NONE', *, *, #6536, .T. ) ;
#510 = EDGE_CURVE ( 'NONE', #9324, #14027, #3441, .T. ) ;
#511 = CARTESIAN_POINT ( 'NONE',  ( 26.49461065740898036, -7.352653653197164019, -5.783357778048668685 ) ) ;
#512 = VERTEX_POINT ( 'NONE', #11862 ) ;
#513 = CARTESIAN_POINT ( 'NONE',  ( 33.43363050022580296, -2.127845067243429256, 6.861505862736166250 ) ) ;
#514 = DIRECTION ( 'NONE',  ( 0.000000000000000000, 0.000000000000000000, -1.000000000000000000 ) ) ;
#515 = CARTESIAN_POINT ( 'NONE',  ( 1.500000000000000000, -10.39230484541326405, -3.000000000000000000 ) ) ;
#516 = ORIENTED_EDGE ( 'NONE', *, *, #8838, .F. ) ;
#517 = CARTESIAN_POINT ( 'NONE',  ( 4.000000000000000000, -1.560351142792949064, -0.2242961665059824972 ) ) ;
#518 = CARTESIAN_POINT ( 'NONE',  ( -4.000000000000000000, -1.680125368658796692, -3.016613018637368970 ) ) ;
#519 = ORIENTED_EDGE ( 'NONE', *, *, #4015, .F. ) ;
#520 = CARTESIAN_POINT ( 'NONE',  ( 26.31065902414478686, -7.328232685206446106, -6.312034385895062272 ) ) ;
#521 = CARTESIAN_POINT ( 'NONE',  ( 26.79905070906539777, -3.354278923027479209, -3.283357778048662023 ) ) ;
#522 = CARTESIAN_POINT ( 'NONE',  ( 26.69778786461289855, -6.274106265784127778, -3.283357778048667797 ) ) ;
#523 = VECTOR ( 'NONE', #4783, 1000.000000000000227 ) ;
#524 = DIRECTION ( 'NONE',  ( 1.000000000000000000, 0.000000000000000000, 0.000000000000000000 ) ) ;
#525 = DIRECTION ( 'NONE',  ( -1.000000000000000000, 1.224646799147352714E-16, 0.000000000000000000 ) ) ;
#526 =( NAMED_UNIT ( * ) SI_UNIT ( $, .STERADIAN. ) SOLID_ANGLE_UNIT ( ) );
#527 = CARTESIAN_POINT ( 'NONE',  ( 27.73357241910951743, -6.576412695658750529, -6.861505862736166250 ) ) ;
#528 = EDGE_CURVE ( 'NONE', #12891, #17459, #462, .T. ) ;
#529 = CARTESIAN_POINT ( 'NONE',  ( 25.99533317148741318, -3.650983533393564517, -3.627061608673662008 ) ) ;
#530 = CARTESIAN_POINT ( 'NONE',  ( 32.55182397003001427, -2.661183353387966299, 8.283357778048664244 ) ) ;
#531 = ORIENTED_EDGE ( 'NONE', *, *, #5477, .T. ) ;
#532 = EDGE_CURVE ( 'NONE', #5221, #4376, #13144, .T. ) ;
#533 = CIRCLE ( 'NONE', #11801, 5.000000000000000000 ) ;
#534 = ORIENTED_EDGE ( 'NONE', *, *, #3431, .T. ) ;
#535 = CARTESIAN_POINT ( 'NONE',  ( 33.40301380667672504, -2.758504307001591549, 7.939653947423664704 ) ) ;
#536 = VECTOR ( 'NONE', #17608, 1000.000000000000000 ) ;
#537 = CARTESIAN_POINT ( 'NONE',  ( 33.43363050022580296, -2.127845067243429256, 6.861505862736166250 ) ) ;
#538 = DIRECTION ( 'NONE',  ( -1.000000000000000000, 0.000000000000000000, 0.000000000000000000 ) ) ;
#539 = CARTESIAN_POINT ( 'NONE',  ( -45.50000000000000000, -16.03270077640482683, 5.537981825772250843 ) ) ;
#540 = PLANE ( 'NONE',  #12777 ) ;
#541 = CARTESIAN_POINT ( 'NONE',  ( 33.13163345120441505, -4.045141346131868154, -3.627061608673664672 ) ) ;
#542 = DIRECTION ( 'NONE',  ( -0.1196152422706610735, 0.9928203230275511881, 0.000000000000000000 ) ) ;
#543 = DIRECTION ( 'NONE',  ( -0.000000000000000000, -0.000000000000000000, 1.000000000000000000 ) ) ;
#544 = CARTESIAN_POINT ( 'NONE',  ( 0.000000000000000000, 0.000000000000000000, -10.00000000000000000 ) ) ;
#545 = LINE ( 'NONE', #13055, #3288 ) ;
#546 = ORIENTED_EDGE ( 'NONE', *, *, #3072, .T. ) ;
#547 = AXIS2_PLACEMENT_3D ( 'NONE', #3870, #17861, #15190 ) ;
#548 = VERTEX_POINT ( 'NONE', #6338 ) ;
#549 = EDGE_CURVE ( 'NONE', #13209, #1004, #4526, .T. ) ;
#550 = CARTESIAN_POINT ( 'NONE',  ( 25.62757597683262034, -3.695291012717980994, -7.939653947423660263 ) ) ;
#551 = CARTESIAN_POINT ( 'NONE',  ( 30.88568772756644520, -4.315733451902305617, -3.283357778048664688 ) ) ;
#552 = CARTESIAN_POINT ( 'NONE',  ( -4.000000000000000000, -2.309401076758508253, -4.700000000000000178 ) ) ;
#553 = CARTESIAN_POINT ( 'NONE',  ( 4.204015924366189871, -1.626724848190929551, -3.310627190413393262 ) ) ;
#554 = ORIENTED_EDGE ( 'NONE', *, *, #8603, .F. ) ;
#555 = CYLINDRICAL_SURFACE ( 'NONE', #10636, 2.500000000000001776 ) ;
#556 = CARTESIAN_POINT ( 'NONE',  ( 29.67353201968042598, -1.554147106732884920, 5.783357778048668685 ) ) ;
#557 = EDGE_CURVE ( 'NONE', #11479, #14024, #4933, .T. ) ;
#558 = VERTEX_POINT ( 'NONE', #17253 ) ;
#559 = CARTESIAN_POINT ( 'NONE',  ( 32.54050588463559990, -2.235448945602741766, -6.861505862736159145 ) ) ;
#560 = ORIENTED_EDGE ( 'NONE', *, *, #7764, .T. ) ;
#561 = VECTOR ( 'NONE', #15631, 1000.000000000000114 ) ;
#562 = EDGE_CURVE ( 'NONE', #5268, #9522, #10410, .T. ) ;
#563 = CARTESIAN_POINT ( 'NONE',  ( 3.248936832696173393, 17.78798921770683350, 17.00000000000000000 ) ) ;
#564 = ORIENTED_EDGE ( 'NONE', *, *, #6190, .F. ) ;
#565 = CARTESIAN_POINT ( 'NONE',  ( 26.63030083514515312, -6.709335133632020387, -6.861505862736167138 ) ) ;
#566 = CARTESIAN_POINT ( 'NONE',  ( 27.89118264539014547, -6.557423775948280742, -6.861505862736167138 ) ) ;
#567 = VECTOR ( 'NONE', #13806, 1000.000000000000227 ) ;
#568 = ORIENTED_EDGE ( 'NONE', *, *, #9077, .T. ) ;
#569 = ADVANCED_FACE ( 'NONE', ( #15869 ), #11769, .T. ) ;
#570 = CARTESIAN_POINT ( 'NONE',  ( 27.51889869220010354, -3.467423976192371082, -7.939653947423660263 ) ) ;
#571 = DIRECTION ( 'NONE',  ( 1.000000000000000000, 0.000000000000000000, -0.000000000000000000 ) ) ;
#572 = CARTESIAN_POINT ( 'NONE',  ( 33.52375369703867847, -2.544085015380856518, -8.283357778048660691 ) ) ;
#573 = DIRECTION ( 'NONE',  ( 0.000000000000000000, 0.000000000000000000, 1.000000000000000000 ) ) ;
#574 = CARTESIAN_POINT ( 'NONE',  ( 27.65467808709180630, -4.705006306174339237, -3.283357778048664688 ) ) ;
#575 = VECTOR ( 'NONE', #16775, 1000.000000000000000 ) ;
#576 = DIRECTION ( 'NONE',  ( -0.9928203230275510771, -0.1196152422706614760, -0.000000000000000000 ) ) ;
#577 = CARTESIAN_POINT ( 'NONE',  ( 26.69778786461289855, -6.274106265784127778, 8.283357778048658915 ) ) ;
#578 = EDGE_CURVE ( 'NONE', #729, #4780, #14420, .T. ) ;
#579 = VERTEX_POINT ( 'NONE', #6435 ) ;
#580 = CARTESIAN_POINT ( 'NONE',  ( 26.31065902414478330, -7.328232685206446106, -6.312034385895062272 ) ) ;
#581 = CARTESIAN_POINT ( 'NONE',  ( -1.654252653721908661, -3.663718938583020446, -0.01223254789874225583 ) ) ;
#582 = EDGE_LOOP ( 'NONE', ( #8490, #11002, #7089, #14364 ) ) ;
#583 = DIRECTION ( 'NONE',  ( 0.9928203230275510771, 0.1196152422706610596, 9.614813431917826478E-17 ) ) ;
#584 = ORIENTED_EDGE ( 'NONE', *, *, #1543, .T. ) ;
#585 = AXIS2_PLACEMENT_3D ( 'NONE', #12458, #11078, #6662 ) ;
#586 = PLANE ( 'NONE',  #16874 ) ;
#587 = CARTESIAN_POINT ( 'NONE',  ( 39.99999999999999289, 2.516649172247811061E-16, -2.055000000000000160 ) ) ;
#588 = CARTESIAN_POINT ( 'NONE',  ( 29.81239362717914787, -2.264323817775507397, -4.533357778048659803 ) ) ;
#589 = CARTESIAN_POINT ( 'NONE',  ( 27.89480254248674740, -2.495355674045408367, -7.033357778048658027 ) ) ;
#590 = LINE ( 'NONE', #17666, #6969 ) ;
#592 = EDGE_CURVE ( 'NONE', #15079, #14461, #13323, .T. ) ;
#591 = PRESENTATION_LAYER_ASSIGNMENT (  '', '', ( #2627 ) ) ;
#593 = CARTESIAN_POINT ( 'NONE',  ( 25.71748644841968456, -2.420320648352046078, 5.783357778048663356 ) ) ;
#594 = CIRCLE ( 'NONE', #15644, 2.500000000000000444 ) ;
#595 = CARTESIAN_POINT ( 'NONE',  ( 33.24613200752366282, -6.212066908601060256, -7.033357778048666908 ) ) ;
#596 = DIRECTION ( 'NONE',  ( -0.1196152422706610735, 0.9928203230275511881, 0.000000000000000000 ) ) ;
#597 = CARTESIAN_POINT ( 'NONE',  ( 33.75714020991769360, -6.487859128256952879, 6.453230759126468818 ) ) ;
#598 = CARTESIAN_POINT ( 'NONE',  ( 26.39370705969127684, -2.976016814310973313, 4.705209693361168455 ) ) ;
#599 = STYLED_ITEM ( 'NONE', ( #6343 ), #8978 ) ;
#600 = ORIENTED_EDGE ( 'NONE', *, *, #8612, .T. ) ;
#601 = CARTESIAN_POINT ( 'NONE',  ( 1.296864337298335788E-21, -1.182044466681725685E-21, -6.899999999999998579 ) ) ;
#602 = VERTEX_POINT ( 'NONE', #10501 ) ;
#603 = EDGE_CURVE ( 'NONE', #11660, #14159, #14693, .T. ) ;
#604 = CARTESIAN_POINT ( 'NONE',  ( 32.30426898124760982, -6.025734024055190652, 4.705209693361159573 ) ) ;
#605 = CARTESIAN_POINT ( 'NONE',  ( -23.43428999263575818, -9.970190943884908563, 14.83168556311182940 ) ) ;
#606 = DIRECTION ( 'NONE',  ( 0.4999999999999921174, -0.8660254037844432595, -0.000000000000000000 ) ) ;
#607 = AXIS2_PLACEMENT_3D ( 'NONE', #12704, #14260, #1658 ) ;
#608 = EDGE_CURVE ( 'NONE', #17849, #6537, #15603, .T. ) ;
#609 = ORIENTED_EDGE ( 'NONE', *, *, #13028, .F. ) ;
#610 = VECTOR ( 'NONE', #16049, 1000.000000000000000 ) ;
#611 = CARTESIAN_POINT ( 'NONE',  ( 4.000000000000000000, -1.942223658245632256, -0.3516579909967657569 ) ) ;
#612 = FACE_OUTER_BOUND ( 'NONE', #16099, .T. ) ;
#613 = B_SPLINE_CURVE_WITH_KNOTS ( 'NONE', 3,
 ( #7742, #1957, #7477, #13001 ),
 .UNSPECIFIED., .F., .F.,
 ( 4, 4 ),
 ( 4.336808689942017736E-19, 0.0003446252387907799432 ),
 .UNSPECIFIED. ) ;
#614 = DIRECTION ( 'NONE',  ( -4.179998415399335043E-17, -3.469446951953615175E-16, -1.000000000000000000 ) ) ;
#615 = CARTESIAN_POINT ( 'NONE',  ( 33.46007730730551799, -5.886481946178435010, -4.705209693361169343 ) ) ;
#616 = CARTESIAN_POINT ( 'NONE',  ( 33.17094678975809074, -2.159493266760871499, -6.861505862736159145 ) ) ;
#617 = COLOUR_RGB ( '', 0.09019608, 0.27058824, 0.51372549) ;
#618 = DIRECTION ( 'NONE',  ( -0.000000000000000000, 0.000000000000000000, -1.000000000000000000 ) ) ;
#619 = LINE ( 'NONE', #14124, #14477 ) ;
#620 = CARTESIAN_POINT ( 'NONE',  ( 28.98992747081925359, -3.290194058894681639, -3.627061608673662896 ) ) ;
#621 = AXIS2_PLACEMENT_3D ( 'NONE', #3165, #7357, #17152 ) ;
#622 = CARTESIAN_POINT ( 'NONE',  ( 26.85044460880409645, -7.319979551716484067, -5.783357778048668685 ) ) ;
#623 = CARTESIAN_POINT ( 'NONE',  ( 30.72436838703367812, -6.515889623968540434, 4.533357778048659803 ) ) ;
#624 = EDGE_LOOP ( 'NONE', ( #16121, #9146, #14535, #15513, #4650, #17869 ) ) ;
#625 = VERTEX_POINT ( 'NONE', #4973 ) ;
#626 = AXIS2_PLACEMENT_3D ( 'NONE', #4264, #16880, #2897 ) ;
#627 = VERTEX_POINT ( 'NONE', #4279 ) ;
#628 = CARTESIAN_POINT ( 'NONE',  ( 32.72003615946069743, -2.840789625746940938, 3.627061608673666449 ) ) ;
#629 = ADVANCED_FACE ( 'NONE', ( #5533 ), #13348, .F. ) ;
#630 = FACE_OUTER_BOUND ( 'NONE', #1139, .T. ) ;
#631 = CARTESIAN_POINT ( 'NONE',  ( -27.17934203385504333, -30.00000000000000355, 13.93658524716016878 ) ) ;
#633 = AXIS2_PLACEMENT_3D ( 'NONE', #8229, #4240, #15388 ) ;
#632 = CARTESIAN_POINT ( 'NONE',  ( 33.43363050022580296, -2.127845067243429256, -4.705209693361160461 ) ) ;
#634 = CARTESIAN_POINT ( 'NONE',  ( 5.781152949374520844, -1.605699403978932294, -1.901951201008075243 ) ) ;
#635 = CIRCLE ( 'NONE', #9875, 3.999999999999998224 ) ;
#636 = CARTESIAN_POINT ( 'NONE',  ( 11.20128062458870843, 15.41171339406673546, 16.67750984750043486 ) ) ;
#637 = CARTESIAN_POINT ( 'NONE',  ( 26.31284730449749532, -7.327874027665321144, -6.311983372246984914 ) ) ;
#638 = UNCERTAINTY_MEASURE_WITH_UNIT (LENGTH_MEASURE( 1.000000000000000082E-05 ), #792, 'distance_accuracy_value', 'NONE');
#639 = CARTESIAN_POINT ( 'NONE',  ( 26.01652455409633902, -4.902371455920926380, 5.783357778048663356 ) ) ;
#640 = EDGE_CURVE ( 'NONE', #12566, #987, #8142, .T. ) ;
#641 = ORIENTED_EDGE ( 'NONE', *, *, #16806, .F. ) ;
#642 = VECTOR ( 'NONE', #3914, 1000.000000000000000 ) ;
#643 = ORIENTED_EDGE ( 'NONE', *, *, #10821, .T. ) ;
#644 = CARTESIAN_POINT ( 'NONE',  ( 26.46816385032927599, -3.594016774262162706, -3.627061608673662896 ) ) ;
#645 = CARTESIAN_POINT ( 'NONE',  ( 31.34233605952372415, -6.778795339760710803, -5.783357778048663356 ) ) ;
#646 = DIRECTION ( 'NONE',  ( 0.9928203230275512992, 0.1196152422706614898, -0.000000000000000000 ) ) ;
#647 = CARTESIAN_POINT ( 'NONE',  ( 26.52132749406794687, -1.933925500942234921, 5.783357778048668685 ) ) ;
#648 = AXIS2_PLACEMENT_3D ( 'NONE', #5014, #7832, #13096 ) ;
#649 = ORIENTED_EDGE ( 'NONE', *, *, #16525, .F. ) ;
#650 = CARTESIAN_POINT ( 'NONE',  ( 29.08935247050201767, -2.014077381790315702, -5.783357778048658027 ) ) ;
#651 = CARTESIAN_POINT ( 'NONE',  ( 30.65370992780335868, -5.597623261208692469, -3.627061608673667781 ) ) ;
#652 = ORIENTED_EDGE ( 'NONE', *, *, #11187, .T. ) ;
#653 = VECTOR ( 'NONE', #15551, 1000.000000000000000 ) ;
#654 = EDGE_CURVE ( 'NONE', #11172, #12535, #8280, .T. ) ;
#655 = CARTESIAN_POINT ( 'NONE',  ( 29.97449477918272009, -6.943593201308171814, -5.113484796970856117 ) ) ;
#656 = CARTESIAN_POINT ( 'NONE',  ( 25.76466184735054910, -2.811881907026620553, -6.248149982130924762 ) ) ;
#657 = LINE ( 'NONE', #7724, #6382 ) ;
#658 = CARTESIAN_POINT ( 'NONE',  ( 4.236525418537981480, -2.416953631397932956, -3.451298686683626826 ) ) ;
#659 = EDGE_CURVE ( 'NONE', #16901, #17078, #11601, .T. ) ;
#660 = CARTESIAN_POINT ( 'NONE',  ( 25.60565592828815440, -3.070961412863312034, -6.861505862736159145 ) ) ;
#661 = DIRECTION ( 'NONE',  ( 0.9928203230275511881, 0.1196152422706614760, 0.000000000000000000 ) ) ;
#662 = CARTESIAN_POINT ( 'NONE',  ( 27.21934464581372737, -3.303641803799556964, -8.283357778048660691 ) ) ;
#663 = CARTESIAN_POINT ( 'NONE',  ( 26.31556265977298992, -7.384422263489805793, -5.783357778048663356 ) ) ;
#664 = CARTESIAN_POINT ( 'NONE',  ( 27.15176839919044482, -1.857969822100365098, -5.783357778048658027 ) ) ;
#665 = DIRECTION ( 'NONE',  ( -1.000000000000000000, 0.000000000000000000, 0.000000000000000000 ) ) ;
#666 = CARTESIAN_POINT ( 'NONE',  ( 31.49429780130001433, -5.496349022752856861, 3.627061608673662896 ) ) ;
#667 = VECTOR ( 'NONE', #5113, 1000.000000000000000 ) ;
#668 =( BOUNDED_CURVE ( )  B_SPLINE_CURVE ( 2, ( #3728, #6807, #10599, #14882, #17820, #3994, #2388, #2468, #7905 ),
 .UNSPECIFIED., .F., .T. ) 
 B_SPLINE_CURVE_WITH_KNOTS ( ( 3, 2, 2, 2, 3 ),
 ( 0.5961538461538461453, 0.6025641025641025328, 0.6153846153846154188, 0.6282051282051281937, 0.6346153846153846922 ),
 .UNSPECIFIED. ) 
 CURVE ( )  GEOMETRIC_REPRESENTATION_ITEM ( )  RATIONAL_B_SPLINE_CURVE ( ( 0.9330127018922194093, 0.9330127018922194093, 1.000000000000000000, 0.8660254037844387076, 1.000000000000000000, 0.8660254037844387076, 1.000000000000000000, 0.9330127018922187432, 0.9330127018922192983 ) ) 
 REPRESENTATION_ITEM ( '' )  );
#669 = ORIENTED_EDGE ( 'NONE', *, *, #13024, .T. ) ;
#670 = CARTESIAN_POINT ( 'NONE',  ( 30.45035428628836627, -2.914368949527523789, -8.283357778048660691 ) ) ;
#671 = LINE ( 'NONE', #11716, #14501 ) ;
#672 = CARTESIAN_POINT ( 'NONE',  ( 33.78529456515154550, -6.484467084455913799, -5.783357778048663356 ) ) ;
#673 = ORIENTED_EDGE ( 'NONE', *, *, #12629, .T. ) ;
#674 = LINE ( 'NONE', #6104, #12815 ) ;
#675 = DIRECTION ( 'NONE',  ( 0.000000000000000000, 0.000000000000000000, 1.000000000000000000 ) ) ;
#676 = DIRECTION ( 'NONE',  ( 1.000000000000000000, 0.000000000000000000, -0.000000000000000000 ) ) ;
#677 = CARTESIAN_POINT ( 'NONE',  ( -25.07353123778395343, 1.235291682954730463, 14.60266621045499669 ) ) ;
#678 = CARTESIAN_POINT ( 'NONE',  ( 33.18300801526289234, -6.557030719496743210, 5.113484796970852564 ) ) ;
#679 = EDGE_LOOP ( 'NONE', ( #8536, #10466 ) ) ;
#680 = CARTESIAN_POINT ( 'NONE',  ( 28.76917853929504432, -3.116917426439186123, -3.283357778048662023 ) ) ;
#681 = DIRECTION ( 'NONE',  ( 0.000000000000000000, 3.469446951953614189E-16, -1.000000000000000000 ) ) ;
#682 = CONTEXT_DEPENDENT_SHAPE_REPRESENTATION ( #16202, #10822 ) ;
#683 = LINE ( 'NONE', #769, #6632 ) ;
#684 = ORIENTED_EDGE ( 'NONE', *, *, #3431, .F. ) ;
#685 = CARTESIAN_POINT ( 'NONE',  ( 30.60986983071443390, -4.348964061499348333, -3.627061608673664672 ) ) ;
#686 = EDGE_CURVE ( 'NONE', #133, #7467, #16259, .T. ) ;
#687 = CARTESIAN_POINT ( 'NONE',  ( 27.42949161418789217, -3.278323244185609830, -3.283357778048662023 ) ) ;
#688 = DIRECTION ( 'NONE',  ( 0.000000000000000000, 0.000000000000000000, 1.000000000000000000 ) ) ;
#689 = VECTOR ( 'NONE', #8945, 999.9999999999998863 ) ;
#690 = CARTESIAN_POINT ( 'NONE',  ( 27.14244485254070938, -4.766720295129625029, 3.627061608673664228 ) ) ;
#691 = SHAPE_REPRESENTATION ( 'MirrorCaliper Body Half', ( #3575 ), #16530 ) ;
#692 = VERTEX_POINT ( 'NONE', #9969 ) ;
#693 = CARTESIAN_POINT ( 'NONE',  ( 27.50150540219088313, -5.977401655418042914, -3.627061608673667781 ) ) ;
#694 = ORIENTED_EDGE ( 'NONE', *, *, #968, .F. ) ;
#695 = CARTESIAN_POINT ( 'NONE',  ( 26.47269060886452507, -6.728324053342490174, 4.705209693361160461 ) ) ;
#696 = CARTESIAN_POINT ( 'NONE',  ( -24.62787796620740011, -10.18046270510853368, 14.56338605435095701 ) ) ;
#697 = CARTESIAN_POINT ( 'NONE',  ( -2.000000000000005329, -3.464101615137750390, 0.000000000000000000 ) ) ;
#698 = EDGE_CURVE ( 'NONE', #6225, #6735, #15073, .T. ) ;
#699 = ORIENTED_EDGE ( 'NONE', *, *, #2456, .F. ) ;
#700 = CARTESIAN_POINT ( 'NONE',  ( 2.500000000000000000, 0.000000000000000000, -10.00000000000000000 ) ) ;
#701 = CARTESIAN_POINT ( 'NONE',  ( 20.25000000000000711, -16.21813761408365195, 13.00000000000000178 ) ) ;
#702 = DIRECTION ( 'NONE',  ( 0.1196152422706618645, -0.9928203230275510771, 0.000000000000000000 ) ) ;
#703 = CARTESIAN_POINT ( 'NONE',  ( 16.75000000000000000, -16.21813761408365195, -16.03574476417184513 ) ) ;
#704 = CARTESIAN_POINT ( 'NONE',  ( 33.38562051666750818, -5.268481986227246061, -7.939653947423664704 ) ) ;
#705 = DIRECTION ( 'NONE',  ( 0.000000000000000000, 1.000000000000000000, -1.287488025362403787E-15 ) ) ;
#706 = CYLINDRICAL_SURFACE ( 'NONE', #12142, 2.499999999999999112 ) ;
#707 = CARTESIAN_POINT ( 'NONE',  ( 27.93049598394382116, -4.671775696577297410, -3.627061608673664672 ) ) ;
#708 = ORIENTED_EDGE ( 'NONE', *, *, #6551, .F. ) ;
#709 = ADVANCED_FACE ( 'NONE', ( #11224 ), #11887, .F. ) ;
#710 = EDGE_CURVE ( 'NONE', #12766, #3366, #5509, .T. ) ;
#711 = CARTESIAN_POINT ( 'NONE',  ( 32.69820532807177216, -4.097360875439379768, -3.283357778048664688 ) ) ;
#712 = CARTESIAN_POINT ( 'NONE',  ( 30.38277803966508372, -1.468696967828331701, 5.783357778048668685 ) ) ;
#713 = ORIENTED_EDGE ( 'NONE', *, *, #16582, .T. ) ;
#714 = VERTEX_POINT ( 'NONE', #14072 ) ;
#715 = ORIENTED_EDGE ( 'NONE', *, *, #7263, .T. ) ;
#716 = CARTESIAN_POINT ( 'NONE',  ( 26.66018910156667232, -2.644102211984857842, 7.033357778048666020 ) ) ;
#717 = CARTESIAN_POINT ( 'NONE',  ( 32.93018312783485868, -2.815471066132993805, 7.939653947423662927 ) ) ;
#718 = FILL_AREA_STYLE_COLOUR ( '', #818 ) ;
#719 = CARTESIAN_POINT ( 'NONE',  ( 0.000000000000000000, 0.000000000000000000, -4.700000000000000178 ) ) ;
#720 = CARTESIAN_POINT ( 'NONE',  ( -18.31859240410168255, -20.37927276054855596, -15.79761704335050077 ) ) ;
#721 = CARTESIAN_POINT ( 'NONE',  ( 32.06767520579373354, -2.292415704734142690, -6.861505862736158257 ) ) ;
#722 = CARTESIAN_POINT ( 'NONE',  ( 29.08935247050201767, -2.014077381790315702, 5.783357778048667797 ) ) ;
#723 = LINE ( 'NONE', #1918, #13063 ) ;
#724 =( BOUNDED_CURVE ( )  B_SPLINE_CURVE ( 2, ( #2368, #1077, #16328, #7886, #2524, #10922, #2617, #16488, #13677 ),
 .UNSPECIFIED., .F., .T. ) 
 B_SPLINE_CURVE_WITH_KNOTS ( ( 3, 2, 2, 2, 3 ),
 ( 0.5576923076923077094, 0.5641025641025640969, 0.5769230769230768718, 0.5897435897435897578, 0.5961538461538461453 ),
 .UNSPECIFIED. ) 
 CURVE ( )  GEOMETRIC_REPRESENTATION_ITEM ( )  RATIONAL_B_SPLINE_CURVE ( ( 0.9330127018922194093, 0.9330127018922194093, 1.000000000000000000, 0.8660254037844387076, 1.000000000000000000, 0.8660254037844387076, 1.000000000000000000, 0.9330127018922194093, 0.9330127018922194093 ) ) 
 REPRESENTATION_ITEM ( '' )  );
#725 = DIRECTION ( 'NONE',  ( 0.000000000000000000, 1.000000000000000000, 0.000000000000000000 ) ) ;
#726 = CARTESIAN_POINT ( 'NONE',  ( 31.32102116884452414, -5.717097954277069682, -8.283357778048664244 ) ) ;
#727 = CARTESIAN_POINT ( 'NONE',  ( 19.91392456697921531, -10.76755109436559010, 15.52754005891982736 ) ) ;
#728 = ORIENTED_EDGE ( 'NONE', *, *, #15440, .F. ) ;
#729 = VERTEX_POINT ( 'NONE', #6905 ) ;
#730 = CARTESIAN_POINT ( 'NONE',  ( 27.62849893492243325, -6.589071975465733644, -4.705209693361168455 ) ) ;
#731 = CARTESIAN_POINT ( 'NONE',  ( 33.76207435632690590, -3.969185667289998332, -3.627061608673664672 ) ) ;
#732 = ORIENTED_EDGE ( 'NONE', *, *, #3449, .F. ) ;
#733 = CARTESIAN_POINT ( 'NONE',  ( 25.92467471225709374, -2.732717170633701453, 4.533357778048667797 ) ) ;
#734 = ADVANCED_FACE ( 'NONE', ( #15433 ), #10728, .F. ) ;
#735 = CARTESIAN_POINT ( 'NONE',  ( 27.96989853965305528, -4.667028466753395222, 3.283357778048664244 ) ) ;
#736 = EDGE_LOOP ( 'NONE', ( #2850, #16797, #4603, #10052 ) ) ;
#737 = CARTESIAN_POINT ( 'NONE',  ( 26.31128205117621022, -7.047579375861630524, 4.533357778048659803 ) ) ;
#738 = EDGE_CURVE ( 'NONE', #16186, #6854, #2363, .T. ) ;
#739 = CARTESIAN_POINT ( 'NONE',  ( 30.25080928106424594, -3.138282701210941994, -3.627061608673662896 ) ) ;
#740 = ORIENTED_EDGE ( 'NONE', *, *, #17456, .F. ) ;
#741 = CARTESIAN_POINT ( 'NONE',  ( 2.500000000000000000, 2.357898499370432166, -2.385244779468109755E-15 ) ) ;
#742 = CARTESIAN_POINT ( 'NONE',  ( 45.50000000000000000, -16.03270077640482683, -8.287981825772241962 ) ) ;
#743 = DIRECTION ( 'NONE',  ( 0.000000000000000000, 0.000000000000000000, -1.000000000000000000 ) ) ;
#744 = FACE_OUTER_BOUND ( 'NONE', #10937, .T. ) ;
#745 = CARTESIAN_POINT ( 'NONE',  ( 27.65911562847151117, -5.958412735707574015, -3.627061608673668225 ) ) ;
#746 = ORIENTED_EDGE ( 'NONE', *, *, #9165, .F. ) ;
#747 = CARTESIAN_POINT ( 'NONE',  ( 27.47505859511117521, -2.218764776483033163, -5.783357778048658027 ) ) ;
#748 = PLANE ( 'NONE',  #4098 ) ;
#749 = LINE ( 'NONE', #17278, #4040 ) ;
#750 = DIRECTION ( 'NONE',  ( -0.000000000000000000, -0.000000000000000000, 1.000000000000000000 ) ) ;
#751 = CARTESIAN_POINT ( 'NONE',  ( 26.52132749406794687, -1.933925500942234921, -5.783357778048658027 ) ) ;
#752 = EDGE_CURVE ( 'NONE', #1869, #2438, #6375, .T. ) ;
#753 = CARTESIAN_POINT ( 'NONE',  ( 31.91006497951310550, -2.311404624444611589, -6.861505862736159145 ) ) ;
#754 = ORIENTED_EDGE ( 'NONE', *, *, #7062, .T. ) ;
#755 = ADVANCED_BREP_SHAPE_REPRESENTATION ( '', ( #5266, #3575 ), #16530 ) ;
#756 = EDGE_CURVE ( 'NONE', #1298, #13310, #2088, .T. ) ;
#757 = VERTEX_POINT ( 'NONE', #7191 ) ;
#758 = CARTESIAN_POINT ( 'NONE',  ( -4.211140560182196957, 2.431303136016540911, -3.445885042887435468 ) ) ;
#759 = CARTESIAN_POINT ( 'NONE',  ( 2.682243648011665371, 3.070208061305305769, -0.04852650426601385486 ) ) ;
#760 = DIRECTION ( 'NONE',  ( 0.000000000000000000, 0.000000000000000000, -1.000000000000000000 ) ) ;
#761 = VERTEX_POINT ( 'NONE', #2823 ) ;
#762 = LINE ( 'NONE', #10269, #2689 ) ;
#763 = FACE_BOUND ( 'NONE', #1135, .T. ) ;
#764 = CARTESIAN_POINT ( 'NONE',  ( -4.281152949374478212, 4.203775615332272508, -3.000000000000000888 ) ) ;
#765 = CARTESIAN_POINT ( 'NONE',  ( 32.04575515724927470, -1.668086104879473730, -5.783357778048658915 ) ) ;
#766 = CARTESIAN_POINT ( 'NONE',  ( 29.94002636988270538, -4.429666970165102136, 3.283357778048664244 ) ) ;
#767 = CARTESIAN_POINT ( 'NONE',  ( 27.95866967485789090, -6.122194908100387245, -3.283357778048667797 ) ) ;
#768 = CARTESIAN_POINT ( 'NONE',  ( -4.211140560182196957, -2.431303136016548017, -3.445885042887436356 ) ) ;
#769 = CARTESIAN_POINT ( 'NONE',  ( 4.000000000000000000, 0.000000000000000000, 13.31572692736085095 ) ) ;
#770 = CYLINDRICAL_SURFACE ( 'NONE', #14705, 12.50000000000000000 ) ;
#771 = CARTESIAN_POINT ( 'NONE',  ( 31.65190802758064592, -5.477360103042387074, -7.939653947423664704 ) ) ;
#772 = ADVANCED_FACE ( 'NONE', ( #7001 ), #5619, .F. ) ;
#773 = DIRECTION ( 'NONE',  ( 0.9928203230275510771, 0.1196152422706609902, 4.006172263299092517E-17 ) ) ;
#774 = FACE_OUTER_BOUND ( 'NONE', #2018, .T. ) ;
#775 = CARTESIAN_POINT ( 'NONE',  ( 26.05393439953038381, -7.587479618990243146, 5.036916015667400437 ) ) ;
#776 = ORIENTED_EDGE ( 'NONE', *, *, #8484, .T. ) ;
#777 = CARTESIAN_POINT ( 'NONE',  ( 26.28374211850154296, -7.120308096563227274, 6.686083953656291712 ) ) ;
#778 = EDGE_LOOP ( 'NONE', ( #8349, #2601, #9455, #8775 ) ) ;
#779 = CARTESIAN_POINT ( 'NONE',  ( 33.56062403295735663, -2.739515387291124426, 7.939653947423664704 ) ) ;
#780 = CARTESIAN_POINT ( 'NONE',  ( -20.27735869291019810, -10.58859781672278899, 15.46157951461808189 ) ) ;
#781 = CARTESIAN_POINT ( 'NONE',  ( 31.26353094466156080, -6.788289799823394866, -5.783357778048663356 ) ) ;
#782 = EDGE_LOOP ( 'NONE', ( #7919, #8135, #1228, #9710 ) ) ;
#783 = CARTESIAN_POINT ( 'NONE',  ( 3.999999999999998224, -2.309401076758513582, -0.5000000000000000000 ) ) ;
#784 = CARTESIAN_POINT ( 'NONE',  ( 30.66124439477291475, -6.860853434864224276, 5.113484796970852564 ) ) ;
#785 = EDGE_CURVE ( 'NONE', #4502, #14075, #17606, .T. ) ;
#786 = DIRECTION ( 'NONE',  ( 0.000000000000000000, -0.000000000000000000, 1.000000000000000000 ) ) ;
#787 = CARTESIAN_POINT ( 'NONE',  ( -3.333333333333334370, 2.694301256218252671, -3.000726591567082213 ) ) ;
#788 = PRODUCT_DEFINITION_FORMATION_WITH_SPECIFIED_SOURCE ( 'ANY', '', #8245, .NOT_KNOWN. ) ;
#789 = CARTESIAN_POINT ( 'NONE',  ( 31.91459173804834748, -5.445711903524953712, -3.627061608673667781 ) ) ;
#790 = CARTESIAN_POINT ( 'NONE',  ( 31.04700706809921940, -2.115577279836057922, 4.533357778048667797 ) ) ;
#791 = LINE ( 'NONE', #6320, #11242 ) ;
#792 =( LENGTH_UNIT ( ) NAMED_UNIT ( * ) SI_UNIT ( .MILLI., .METRE. ) );
#793 = CARTESIAN_POINT ( 'NONE',  ( 28.23249303296521617, -2.754479417688857179, -4.705209693361161349 ) ) ;
#794 = CIRCLE ( 'NONE', #17025, 2.500000000000000888 ) ;
#795 = ADVANCED_FACE ( 'NONE', ( #4080 ), #8157, .T. ) ;
#796 = CARTESIAN_POINT ( 'NONE',  ( 31.98525019727866692, -6.363978266284800789, 4.533357778048659803 ) ) ;
#797 = ORIENTED_EDGE ( 'NONE', *, *, #6971, .F. ) ;
#798 = ORIENTED_EDGE ( 'NONE', *, *, #7563, .F. ) ;
#799 = ORIENTED_EDGE ( 'NONE', *, *, #2607, .T. ) ;
#800 = CARTESIAN_POINT ( 'NONE',  ( 26.35439372113758694, -4.861664893681965083, 3.627061608673664228 ) ) ;
#801 = CARTESIAN_POINT ( 'NONE',  ( 32.06767520579373354, -2.292415704734142690, 4.705209693361168455 ) ) ;
#802 = AXIS2_PLACEMENT_3D ( 'NONE', #6740, #12276, #16535 ) ;
#803 = CARTESIAN_POINT ( 'NONE',  ( 32.47301885516785092, -2.670677813450649918, 8.283357778048666020 ) ) ;
#804 = EDGE_CURVE ( 'NONE', #14976, #15476, #12782, .T. ) ;
#805 = CARTESIAN_POINT ( 'NONE',  ( -16.96458082634299558, -17.85487492059188597, -16.00470661676384054 ) ) ;
#806 = CARTESIAN_POINT ( 'NONE',  ( 29.55043834383899437, -5.730545699181964991, -3.627061608673668225 ) ) ;
#807 = DIRECTION ( 'NONE',  ( 0.000000000000000000, 0.000000000000000000, 1.000000000000000000 ) ) ;
#808 = CARTESIAN_POINT ( 'NONE',  ( 32.61569110240115776, -6.288022587442930522, -7.033357778048666908 ) ) ;
#809 = CARTESIAN_POINT ( 'NONE',  ( 31.34233605952372415, -6.778795339760710803, -5.783357778048663356 ) ) ;
#810 = CARTESIAN_POINT ( 'NONE',  ( 30.00264913441657555, -6.940201157507134511, -5.783357778048657138 ) ) ;
#811 =( NAMED_UNIT ( * ) SI_UNIT ( $, .STERADIAN. ) SOLID_ANGLE_UNIT ( ) );
#812 = ORIENTED_EDGE ( 'NONE', *, *, #12281, .T. ) ;
#813 = CARTESIAN_POINT ( 'NONE',  ( 33.35047706458318828, -2.764833946905071560, -7.939653947423660263 ) ) ;
#814 = CARTESIAN_POINT ( 'NONE',  ( 33.33308377457396432, -5.274811626130743392, -3.627061608673668225 ) ) ;
#815 = EDGE_LOOP ( 'NONE', ( #969, #7998, #5616, #17835 ) ) ;
#816 = CARTESIAN_POINT ( 'NONE',  ( 1.999999999999997113, -3.464101615137767265, -2.842992957459238301 ) ) ;
#817 = PRODUCT_DEFINITION ( 'UNKNOWN', '', #4819, #12962 ) ;
#818 = COLOUR_RGB ( '', 0.09019608, 0.27058824, 0.51372549) ;
#819 = CARTESIAN_POINT ( 'NONE',  ( -7.958171371210956302, 6.326703190994831694, -2.666481567098320404 ) ) ;
#820 = AXIS2_PLACEMENT_3D ( 'NONE', #12110, #886, #3877 ) ;
#821 = EDGE_LOOP ( 'NONE', ( #12913, #198, #11384, #8365 ) ) ;
#822 = CARTESIAN_POINT ( 'NONE',  ( 26.31065902414478686, -7.328232685206446106, 5.254681170202263552 ) ) ;
#823 = AXIS2_PLACEMENT_3D ( 'NONE', #191, #1650, #1838 ) ;
#824 = CARTESIAN_POINT ( 'NONE',  ( 31.53813789838894621, -6.745008222462202774, -5.783357778048668685 ) ) ;
#825 = VERTEX_POINT ( 'NONE', #13523 ) ;
#826 = EDGE_CURVE ( 'NONE', #11736, #17680, #13359, .T. ) ;
#827 = CARTESIAN_POINT ( 'NONE',  ( 7.499998387031003411, -20.49508120620799900, 13.00000000000000178 ) ) ;
#828 = CARTESIAN_POINT ( 'NONE',  ( 31.00199007654869732, -2.847907730748336697, -8.283357778048660691 ) ) ;
#829 = EDGE_CURVE ( 'NONE', #397, #17258, #16253, .T. ) ;
#830 = DIRECTION ( 'NONE',  ( 0.000000000000000000, 0.000000000000000000, 1.000000000000000000 ) ) ;
#831 = CIRCLE ( 'NONE', #13854, 2.100000000000000089 ) ;
#832 = DIRECTION ( 'NONE',  ( 1.000000000000000000, 0.000000000000000000, 0.000000000000000000 ) ) ;
#833 = UNCERTAINTY_MEASURE_WITH_UNIT (LENGTH_MEASURE( 1.000000000000000082E-05 ), #16057, 'distance_accuracy_value', 'NONE');
#834 = B_SPLINE_CURVE_WITH_KNOTS ( 'NONE', 3,
 ( #13075, #6361, #11976, #3651, #9089 ),
 .UNSPECIFIED., .F., .F.,
 ( 4, 1, 4 ),
 ( 0.000000000000000000, 0.002309401076758504923, 0.004618802153517009845 ),
 .UNSPECIFIED. ) ;
#835 = CARTESIAN_POINT ( 'NONE',  ( 32.47301885516785092, -2.670677813450649474, -3.283357778048662023 ) ) ;
#836 = CARTESIAN_POINT ( 'NONE',  ( 26.99805802979993885, -6.665027654307603022, -4.705209693361168455 ) ) ;
#837 = EDGE_CURVE ( 'NONE', #7608, #1468, #5335, .T. ) ;
#838 = CARTESIAN_POINT ( 'NONE',  ( -50.00000000000000000, -16.03270077640482683, -5.537981825772250843 ) ) ;
#839 = CARTESIAN_POINT ( 'NONE',  ( 1.274241539467174222, 3.883118457693031544, -2.920601398289339290 ) ) ;
#840 = CARTESIAN_POINT ( 'NONE',  ( 28.64916707261694384, -6.765910400363817523, -4.533357778048668685 ) ) ;
#841 = CARTESIAN_POINT ( 'NONE',  ( 30.88577694472199298, -6.196634301449400084, -6.861505862736166250 ) ) ;
#842 = AXIS2_PLACEMENT_3D ( 'NONE', #9935, #3246, #7424 ) ;
#843 = DIRECTION ( 'NONE',  ( -1.000000000000000000, 0.000000000000000000, 0.000000000000000000 ) ) ;
#844 = CARTESIAN_POINT ( 'NONE',  ( 26.66770885555339987, -3.370103022578743612, -8.283357778048660691 ) ) ;
#845 = CARTESIAN_POINT ( 'NONE',  ( -2.016448651773435938E-27, -20.49999999999999645, 13.00000000000000178 ) ) ;
#846 = ORIENTED_EDGE ( 'NONE', *, *, #2531, .T. ) ;
#847 = DIRECTION ( 'NONE',  ( -0.000000000000000000, 1.000000000000000000, -0.000000000000000000 ) ) ;
#848 = CIRCLE ( 'NONE', #14764, 9.500000000000001776 ) ;
#849 = FACE_OUTER_BOUND ( 'NONE', #85, .T. ) ;
#850 = ADVANCED_FACE ( 'NONE', ( #2547 ), #1096, .T. ) ;
#851 = CARTESIAN_POINT ( 'NONE',  ( 0.000000000000000000, 0.000000000000000000, -3.000000000000002665 ) ) ;
#852 = CARTESIAN_POINT ( 'NONE',  ( 29.79859849048667897, -1.928627242885762705, -5.783357778048664244 ) ) ;
#853 = AXIS2_PLACEMENT_3D ( 'NONE', #5515, #12329, #5425 ) ;
#854 = CARTESIAN_POINT ( 'NONE',  ( 30.25524682244395436, -4.391689130744175884, -3.283357778048664688 ) ) ;
#855 = CYLINDRICAL_SURFACE ( 'NONE', #296, 2.500000000000001776 ) ;
#856 = CONTEXT_DEPENDENT_SHAPE_REPRESENTATION ( #3796, #2596 ) ;
#857 = DIRECTION ( 'NONE',  ( 1.000000000000000000, 0.000000000000000000, 0.000000000000000000 ) ) ;
#858 = DIRECTION ( 'NONE',  ( -0.000000000000000000, -0.000000000000000000, -1.000000000000000000 ) ) ;
#859 = ORIENTED_EDGE ( 'NONE', *, *, #7991, .T. ) ;
#860 = CARTESIAN_POINT ( 'NONE',  ( 30.40841950734487753, -3.119293781500474427, -3.627061608673662008 ) ) ;
#861 = LINE ( 'NONE', #7487, #4406 ) ;
#862 = CARTESIAN_POINT ( 'NONE',  ( 26.18940075748478691, -6.337263906362392341, -7.823530922983556124 ) ) ;
#863 = CARTESIAN_POINT ( 'NONE',  ( 27.65458886993626564, -2.824105456627233224, 4.705209693361168455 ) ) ;
#864 = AXIS2_PLACEMENT_3D ( 'NONE', #2854, #2504, #5472 ) ;
#865 = CIRCLE ( 'NONE', #10967, 4.250000000000000000 ) ;
#866 = ORIENTED_EDGE ( 'NONE', *, *, #16999, .T. ) ;
#867 = VECTOR ( 'NONE', #15936, 1000.000000000000000 ) ;
#868 = EDGE_LOOP ( 'NONE', ( #110, #4824, #5826, #15634 ) ) ;
#869 = CARTESIAN_POINT ( 'NONE',  ( 33.44685390376565692, -4.007163506710925027, 3.627061608673664228 ) ) ;
#870 = CARTESIAN_POINT ( 'NONE',  ( -26.11885528537984413, -10.78654967147420329, 14.20677827292374040 ) ) ;
#871 = DIRECTION ( 'NONE',  ( 0.9928203230275510771, 0.1196152422706614621, -0.000000000000000000 ) ) ;
#872 = EDGE_LOOP ( 'NONE', ( #16482, #13796, #4156, #9248 ) ) ;
#873 = CARTESIAN_POINT ( 'NONE',  ( 32.89331279191618762, -2.620040694222726785, -8.283357778048660691 ) ) ;
#874 = FACE_OUTER_BOUND ( 'NONE', #5971, .T. ) ;
#875 = EDGE_CURVE ( 'NONE', #17192, #6885, #1465, .T. ) ;
#876 = CARTESIAN_POINT ( 'NONE',  ( 28.20260476654369697, -6.819712339336020612, -7.033357778048666908 ) ) ;
#877 = CARTESIAN_POINT ( 'NONE',  ( 32.72003615946069743, -2.840789625746940938, -7.939653947423660263 ) ) ;
#878 =( BOUNDED_CURVE ( )  B_SPLINE_CURVE ( 3, ( #12266, #2658, #4104, #17834 ),
 .UNSPECIFIED., .F., .T. ) 
 B_SPLINE_CURVE_WITH_KNOTS ( ( 4, 4 ),
 ( 4.715434792643774742, 4.769085813125753859 ),
 .UNSPECIFIED. ) 
 CURVE ( )  GEOMETRIC_REPRESENTATION_ITEM ( )  RATIONAL_B_SPLINE_CURVE ( ( 1.000000000000000000, 0.9997601450507493936, 0.9997601450507493936, 1.000000000000000000 ) ) 
 REPRESENTATION_ITEM ( '' )  );
#879 = EDGE_LOOP ( 'NONE', ( #7853, #3390, #4842, #9756 ) ) ;
#880 = CARTESIAN_POINT ( 'NONE',  ( 32.67202617590239555, -5.981426544730773287, -4.705209693361168455 ) ) ;
#881 = CARTESIAN_POINT ( 'NONE',  ( 31.20090818012769773, -4.277755612481361602, 3.283357778048664244 ) ) ;
#882 = CARTESIAN_POINT ( 'NONE',  ( 31.98525019727866692, -6.363978266284800789, -7.033357778048666908 ) ) ;
#883 = EDGE_CURVE ( 'NONE', #15791, #4053, #3323, .T. ) ;
#884 = CARTESIAN_POINT ( 'NONE',  ( 26.97161122272022382, -2.906390775372597712, -4.705209693361161349 ) ) ;
#885 = CARTESIAN_POINT ( 'NONE',  ( 32.47301885516785092, -2.670677813450649918, -3.283357778048662023 ) ) ;
#886 = DIRECTION ( 'NONE',  ( 0.000000000000000000, 1.000000000000000000, 3.469446951953614189E-16 ) ) ;
#887 = CARTESIAN_POINT ( 'NONE',  ( 33.15485366002904755, -6.560422763297783177, -5.783357778048663356 ) ) ;
#888 = CARTESIAN_POINT ( 'NONE',  ( 30.12771560522282499, -7.314681293660012074, 5.783357778048657138 ) ) ;
#889 = ADVANCED_FACE ( 'NONE', ( #8168 ), #13700, .F. ) ;
#890 = ORIENTED_EDGE ( 'NONE', *, *, #2202, .F. ) ;
#891 = CIRCLE ( 'NONE', #10711, 2.749999999999988454 ) ;
#892 = EDGE_LOOP ( 'NONE', ( #16804, #362, #17173, #5580, #7051, #16763, #4405, #6326, #15115, #12241, #12488, #3250, #12215, #13332, #13318, #14853, #7542, #437, #17367, #11537, #17704, #12031, #11724, #1885, #14496, #10853, #684, #7322, #1022 ) ) ;
#893 = EDGE_LOOP ( 'NONE', ( #5361, #16625 ) ) ;
#894 = LINE ( 'NONE', #10494, #523 ) ;
#895 = CARTESIAN_POINT ( 'NONE',  ( 33.46007730730551799, -5.886481946178435010, 6.861505862736157368 ) ) ;
#896 = EDGE_LOOP ( 'NONE', ( #11196, #11197, #11319, #5052 ) ) ;
#897 =( LENGTH_UNIT ( ) NAMED_UNIT ( * ) SI_UNIT ( .MILLI., .METRE. ) );
#898 = AXIS2_PLACEMENT_3D ( 'NONE', #1568, #4458, #11058 ) ;
#899 = DIRECTION ( 'NONE',  ( 0.9928203230275510771, 0.1196152422706610596, 9.614813431917826478E-17 ) ) ;
#900 = CARTESIAN_POINT ( 'NONE',  ( 27.26436163736424945, -2.571311352887278190, -7.033357778048658027 ) ) ;
#901 = CARTESIAN_POINT ( 'NONE',  ( 30.39102621733566423, -5.629271460726126719, -7.939653947423664704 ) ) ;
#902 = CARTESIAN_POINT ( 'NONE',  ( 30.32207992551315812, -1.865558067907615802, -6.453230759126468818 ) ) ;
#903 = CARTESIAN_POINT ( 'NONE',  ( 0.000000000000000000, 0.000000000000000000, 10.50000000000000000 ) ) ;
#904 = CARTESIAN_POINT ( 'NONE',  ( 20.00000000000000355, 7.999999999999996447, 6.000000000000000000 ) ) ;
#905 = CARTESIAN_POINT ( 'NONE',  ( 27.23882169172318513, -6.009049854935478052, -7.939653947423664704 ) ) ;
#906 = VECTOR ( 'NONE', #7722, 1000.000000000000000 ) ;
#907 = CARTESIAN_POINT ( 'NONE',  ( 29.74110826630371207, -2.999819088432076786, -8.283357778048660691 ) ) ;
#908 = ORIENTED_EDGE ( 'NONE', *, *, #9380, .T. ) ;
#909 = VECTOR ( 'NONE', #7982, 1000.000000000000227 ) ;
#910 = CARTESIAN_POINT ( 'NONE',  ( 31.02146712245815507, -5.553315781884258229, -7.939653947423664704 ) ) ;
#911 = CARTESIAN_POINT ( 'NONE',  ( 32.19919549706052209, -6.038393303862174655, -4.705209693361169343 ) ) ;
#912 = ORIENTED_EDGE ( 'NONE', *, *, #15355, .F. ) ;
#913 = CARTESIAN_POINT ( 'NONE',  ( -9.099998387031003944, -19.29508120620799616, -12.00000000000000000 ) ) ;
#914 = CIRCLE ( 'NONE', #1211, 3.000000000000000000 ) ;
#915 = ADVANCED_FACE ( 'NONE', ( #1453 ), #39, .T. ) ;
#916 = CARTESIAN_POINT ( 'NONE',  ( 26.16860980394290692, -3.430234601869349920, 8.283357778048664244 ) ) ;
#917 = ORIENTED_EDGE ( 'NONE', *, *, #307, .T. ) ;
#918 = CARTESIAN_POINT ( 'NONE',  ( 32.77701044293393551, -4.087866415376695706, -3.283357778048664688 ) ) ;
#919 = COLOUR_RGB ( '', 0.40784314, 0.44705882, 0.49803922) ;
#920 = CARTESIAN_POINT ( 'NONE',  ( 33.42946061375642586, -6.517141185936593750, -5.783357778048668685 ) ) ;
#921 = EDGE_LOOP ( 'NONE', ( #12504, #6661, #5208, #15907 ) ) ;
#922 = DIRECTION ( 'NONE',  ( -1.000000000000000000, 0.000000000000000000, 0.000000000000000000 ) ) ;
#923 = CARTESIAN_POINT ( 'NONE',  ( 31.24221605398236079, -5.726592414339752857, -8.283357778048664244 ) ) ;
#924 = CARTESIAN_POINT ( 'NONE',  ( -35.77680296528374271, -19.03270077640483038, 0.5379818257722508434 ) ) ;
#925 = AXIS2_PLACEMENT_3D ( 'NONE', #16168, #3464, #2298 ) ;
#926 = CARTESIAN_POINT ( 'NONE',  ( 1.243833333692658361, -3.900674643482532122, -2.923144239647436304 ) ) ;
#927 = CARTESIAN_POINT ( 'NONE',  ( 30.80688261270428541, -4.325227911964988792, -3.283357778048664688 ) ) ;
#928 = EDGE_LOOP ( 'NONE', ( #13170, #2992, #5507, #9711 ) ) ;
#929 = CARTESIAN_POINT ( 'NONE',  ( 28.14933959732260149, -3.391468297350501260, -7.939653947423660263 ) ) ;
#930 = VECTOR ( 'NONE', #8401, 1000.000000000000227 ) ;
#931 = DIRECTION ( 'NONE',  ( 1.000000000000000000, 0.000000000000000000, 0.000000000000000000 ) ) ;
#932 = FACE_OUTER_BOUND ( 'NONE', #17119, .T. ) ;
#933 = CARTESIAN_POINT ( 'NONE',  ( 20.00000000000000000, 7.999999999999996447, -15.51150668642334374 ) ) ;
#934 = CARTESIAN_POINT ( 'NONE',  ( 28.15758777499317489, -7.552042790248305160, -5.783357778048669573 ) ) ;
#935 = ADVANCED_FACE ( 'NONE', ( #16509 ), #13868, .T. ) ;
#936 = CARTESIAN_POINT ( 'NONE',  ( 30.67110321781257909, -3.087645581983020637, -7.939653947423660263 ) ) ;
#937 = CIRCLE ( 'NONE', #357, 6.000000000000000888 ) ;
#938 = EDGE_CURVE ( 'NONE', #6497, #761, #8426, .T. ) ;
#939 = AXIS2_PLACEMENT_3D ( 'NONE', #15744, #17213, #596 ) ;
#940 = VECTOR ( 'NONE', #5062, 1000.000000000000000 ) ;
#941 = ORIENTED_EDGE ( 'NONE', *, *, #14365, .T. ) ;
#942 = CARTESIAN_POINT ( 'NONE',  ( -35.41536221060850664, -16.03270077640482683, 10.53798182577225084 ) ) ;
#943 = DIRECTION ( 'NONE',  ( -0.9937818688019538493, -0.1113444980252557837, 0.000000000000000000 ) ) ;
#944 = EDGE_LOOP ( 'NONE', ( #3210, #11265, #10421, #10951, #13756 ) ) ;
#945 = CARTESIAN_POINT ( 'NONE',  ( 26.01345249736710841, -4.876873030332669501, 3.385440998859989836 ) ) ;
#947 = VERTEX_POINT ( 'NONE', #13962 ) ;
#946 = CARTESIAN_POINT ( 'NONE',  ( 1.500000000000000000, -11.00000000000000000, -9.708203932499369415 ) ) ;
#948 = CARTESIAN_POINT ( 'NONE',  ( 26.92924972366625980, -7.310485091653801781, -5.783357778048657138 ) ) ;
#949 = DIRECTION ( 'NONE',  ( -0.9928203230275512992, -0.1196152422706610180, -4.006172263299093133E-17 ) ) ;
#950 = AXIS2_PLACEMENT_3D ( 'NONE', #9550, #2681, #10089 ) ;
#951 = AXIS2_PLACEMENT_3D ( 'NONE', #9490, #8145, #8230 ) ;
#952 = CARTESIAN_POINT ( 'NONE',  ( 29.98885399772409954, -6.604504582617394703, -4.533357778048668685 ) ) ;
#953 = FACE_OUTER_BOUND ( 'NONE', #4533, .T. ) ;
#954 = DIRECTION ( 'NONE',  ( 0.000000000000000000, 0.000000000000000000, -1.000000000000000000 ) ) ;
#955 = CARTESIAN_POINT ( 'NONE',  ( -7.499998387031003411, -20.49508120620799900, 12.00000000000000000 ) ) ;
#956 = CARTESIAN_POINT ( 'NONE',  ( 28.71854711534694715, -4.576831098024959132, -3.627061608673664672 ) ) ;
#957 = CARTESIAN_POINT ( 'NONE',  ( 33.19286683830256379, -2.783822866615540903, -7.939653947423660263 ) ) ;
#958 = CARTESIAN_POINT ( 'NONE',  ( 25.76466184735054910, -2.811881907026620553, -6.248149982130924762 ) ) ;
#959 = CARTESIAN_POINT ( 'NONE',  ( 27.15566825608056689, -6.646038734597135011, 6.861505862736157368 ) ) ;
#960 = ORIENTED_EDGE ( 'NONE', *, *, #7086, .F. ) ;
#961 = EDGE_CURVE ( 'NONE', #5034, #5157, #461, .T. ) ;
#962 = STYLED_ITEM ( 'NONE', ( #1134 ), #17490 ) ;
#963 = VERTEX_POINT ( 'NONE', #7084 ) ;
#964 = CIRCLE ( 'NONE', #17508, 10.50000000000000000 ) ;
#965 = CARTESIAN_POINT ( 'NONE',  ( 31.65190802758064592, -5.477360103042387074, 3.627061608673662896 ) ) ;
#966 = CARTESIAN_POINT ( 'NONE',  ( 27.36943512155133362, -2.558652073080304845, 7.033357778048666020 ) ) ;
#967 = LINE ( 'NONE', #8942, #11342 ) ;
#968 = EDGE_CURVE ( 'NONE', #2889, #16703, #5054, .T. ) ;
#969 = ORIENTED_EDGE ( 'NONE', *, *, #6749, .F. ) ;
#970 = CARTESIAN_POINT ( 'NONE',  ( -14.00000000000000178, 0.000000000000000000, -10.50000000000000000 ) ) ;
#971 = DIRECTION ( 'NONE',  ( -0.000000000000000000, -0.000000000000000000, 1.000000000000000000 ) ) ;
#973 = VECTOR ( 'NONE', #7890, 1000.000000000000000 ) ;
#972 = CARTESIAN_POINT ( 'NONE',  ( 39.14763340350798160, -5.210289818862206879, -9.533357778048658915 ) ) ;
#974 = CARTESIAN_POINT ( 'NONE',  ( 33.54323074294813267, -5.249493066516778050, -7.939653947423664704 ) ) ;
#975 = ORIENTED_EDGE ( 'NONE', *, *, #1009, .F. ) ;
#976 = CARTESIAN_POINT ( 'NONE',  ( 32.01513846370018967, -2.298745344637636912, -4.705209693361161349 ) ) ;
#977 = DIRECTION ( 'NONE',  ( 0.000000000000000000, 1.000000000000000000, 0.000000000000000000 ) ) ;
#978 = DIRECTION ( 'NONE',  ( 0.9928203230275511881, 0.1196152422706614482, 0.000000000000000000 ) ) ;
#979 =( LENGTH_UNIT ( ) NAMED_UNIT ( * ) SI_UNIT ( .MILLI., .METRE. ) );
#980 = CARTESIAN_POINT ( 'NONE',  ( 30.08145424927873535, -6.930706697444451336, -5.783357778048663356 ) ) ;
#981 = CARTESIAN_POINT ( 'NONE',  ( 33.06225340847440464, -6.234220648470727433, -4.533357778048668685 ) ) ;
#982 = CARTESIAN_POINT ( 'NONE',  ( 5.500000000000000000, -20.49999999999999645, 6.000000000000000000 ) ) ;
#983 = CARTESIAN_POINT ( 'NONE',  ( 29.08935247050201767, -2.014077381790315702, -5.783357778048658027 ) ) ;
#984 = CARTESIAN_POINT ( 'NONE',  ( 28.16881664323205570, -6.096876348486420127, 3.283357778048663800 ) ) ;
#985 = EDGE_CURVE ( 'NONE', #8671, #5626, #17505, .T. ) ;
#986 = ORIENTED_EDGE ( 'NONE', *, *, #7868, .T. ) ;
#987 = VERTEX_POINT ( 'NONE', #5692 ) ;
#988 = VECTOR ( 'NONE', #8852, 1000.000000000000227 ) ;
#989 = ORIENTED_EDGE ( 'NONE', *, *, #10188, .F. ) ;
#990 = CARTESIAN_POINT ( 'NONE',  ( 33.38562051666750818, -5.268481986227246061, 3.627061608673662896 ) ) ;
#991 = CARTESIAN_POINT ( 'NONE',  ( 31.65190802758064592, -5.477360103042387074, 3.627061608673662896 ) ) ;
#992 = EDGE_CURVE ( 'NONE', #12531, #11629, #15318, .T. ) ;
#993 = ORIENTED_EDGE ( 'NONE', *, *, #16072, .T. ) ;
#994 =( BOUNDED_SURFACE ( )  B_SPLINE_SURFACE ( 3, 2, ( 
 ( #12064, #10687, #6368 ),
 ( #2217, #16265, #14548 ),
 ( #2130, #14636, #10528 ),
 ( #839, #14889, #11891 ),
 ( #17471, #11, #5346 ),
 ( #9433, #4273, #2817 ) ),
 .UNSPECIFIED., .F., .F., .T. ) 
 B_SPLINE_SURFACE_WITH_KNOTS ( ( 4, 2, 4 ),
 ( 3, 3 ),
 ( 0.02023740217035200836, 0.02269762987400599299, 0.02515785757765997763 ),
 ( 0.000000000000000000, 1.000000000000000000 ),
 .UNSPECIFIED. ) 
 GEOMETRIC_REPRESENTATION_ITEM ( )  RATIONAL_B_SPLINE_SURFACE ( (
 ( 1.000000000000000000, 0.8047781539129733597, 1.000000000000000000),
 ( 1.000000000000000000, 0.8123770319056771161, 1.000000000000000000),
 ( 1.000000000000000000, 0.8190663783057344771, 1.000000000000000000),
 ( 1.000000000000000000, 0.8192359702876569338, 1.000000000000000000),
 ( 1.000000000000000000, 0.8126134888420186719, 1.000000000000000000),
 ( 1.000000000000000000, 0.8047712368238110203, 1.000000000000000000) ) ) 
 REPRESENTATION_ITEM ( '' )  SURFACE ( )  );
#995 = CARTESIAN_POINT ( 'NONE',  ( -1.917618200156724081E-28, -7.000000000000001776, 0.000000000000000000 ) ) ;
#996 = CARTESIAN_POINT ( 'NONE',  ( 32.92339180097568629, -5.524043937428110063, 8.283357778048660691 ) ) ;
#997 = CARTESIAN_POINT ( 'NONE',  ( 45.50000000000000000, -19.03270077640483038, -2.787981825772258837 ) ) ;
#998 = CARTESIAN_POINT ( 'NONE',  ( 30.92509028327567933, -4.310986222078405206, -7.939653947423662039 ) ) ;
#999 = CARTESIAN_POINT ( 'NONE',  ( 33.60446413004628141, -3.988174587000466342, 7.939653947423662039 ) ) ;
#1000 = CARTESIAN_POINT ( 'NONE',  ( 31.15208055228630357, -2.102918000029084578, -4.533357778048659803 ) ) ;
#1001 = DIRECTION ( 'NONE',  ( 0.000000000000000000, 0.000000000000000000, -1.000000000000000000 ) ) ;
#1002 = CARTESIAN_POINT ( 'NONE',  ( 26.37178701114681800, -2.351687214456304353, -5.783357778048658027 ) ) ;
#1003 = CARTESIAN_POINT ( 'NONE',  ( 18.32916366311290091, -12.06017896066153128, 15.79554754021495633 ) ) ;
#1004 = VERTEX_POINT ( 'NONE', #12876 ) ;
#1005 = CARTESIAN_POINT ( 'NONE',  ( 32.08959525433819238, -2.916745304588811649, -7.939653947423660263 ) ) ;
#1006 = CARTESIAN_POINT ( 'NONE',  ( 33.44685390376565692, -4.007163506710925027, -7.939653947423662039 ) ) ;
#1007 = ORIENTED_EDGE ( 'NONE', *, *, #1104, .F. ) ;
#1008 = CARTESIAN_POINT ( 'NONE',  ( -30.07408527595751124, -27.82894256842315883, 13.18310524188696853 ) ) ;
#1009 = EDGE_CURVE ( 'NONE', #5050, #17268, #3521, .T. ) ;
#1010 = CARTESIAN_POINT ( 'NONE',  ( 25.89088658894545603, -2.009881179784104965, 5.783357778048668685 ) ) ;
#1011 = PRODUCT_DEFINITION_SHAPE ( 'NONE', 'NONE',  #17974 ) ;
#1012 = VERTEX_POINT ( 'NONE', #15590 ) ;
#1013 = CARTESIAN_POINT ( 'NONE',  ( 30.75425665345519732, -2.450656702321377001, 6.861505862736165362 ) ) ;
#1014 = CARTESIAN_POINT ( 'NONE',  ( 27.49697864365563760, -2.843094376337701679, -6.861505862736159145 ) ) ;
#1015 =( BOUNDED_CURVE ( )  B_SPLINE_CURVE ( 2, ( #2395, #4004, #11890, #2216, #3919, #7910, #7995, #9432, #7729 ),
 .UNSPECIFIED., .F., .T. ) 
 B_SPLINE_CURVE_WITH_KNOTS ( ( 3, 2, 2, 2, 3 ),
 ( 0.1346153846153846367, 0.1410256410256410242, 0.1538461538461538547, 0.1666666666666666574, 0.1730769230769231004 ),
 .UNSPECIFIED. ) 
 CURVE ( )  GEOMETRIC_REPRESENTATION_ITEM ( )  RATIONAL_B_SPLINE_CURVE ( ( 0.9330127018922194093, 0.9330127018922196314, 1.000000000000000000, 0.8660254037844387076, 1.000000000000000000, 0.8660254037844387076, 1.000000000000000000, 0.9330127018922190762, 0.9330127018922194093 ) ) 
 REPRESENTATION_ITEM ( '' )  );
#1016 = CARTESIAN_POINT ( 'NONE',  ( 26.14833026707293939, -5.996374093462653931, -8.004211544232147091 ) ) ;
#1017 = CARTESIAN_POINT ( 'NONE',  ( -13.00000000000000178, -1.592040838891559293E-15, 6.000000000000000000 ) ) ;
#1018 = CARTESIAN_POINT ( 'NONE',  ( 3.436326524993535081, -2.634838109287350516, -3.231543764078689929 ) ) ;
#1019 = EDGE_CURVE ( 'NONE', #12756, #8671, #10603, .T. ) ;
#1020 = CARTESIAN_POINT ( 'NONE',  ( 33.13353876934984754, -5.498725377814142945, -8.283357778048662468 ) ) ;
#1021 =( REPRESENTATION_RELATIONSHIP ('NONE','NONE', #3227, #3339 ) REPRESENTATION_RELATIONSHIP_WITH_TRANSFORMATION ( #9113 )SHAPE_REPRESENTATION_RELATIONSHIP( ) );
#1022 = ORIENTED_EDGE ( 'NONE', *, *, #17303, .T. ) ;
#1023 = CARTESIAN_POINT ( 'NONE',  ( 32.02836186724004364, -4.178063784105134459, -7.939653947423662039 ) ) ;
#1024 = CARTESIAN_POINT ( 'NONE',  ( -13.00000000000000178, 1.592040838891559293E-15, -12.00000000000000000 ) ) ;
#1025 = FACE_OUTER_BOUND ( 'NONE', #3424, .T. ) ;
#1026 = CARTESIAN_POINT ( 'NONE',  ( 18.99795248260418745, 9.336063356527739998, -15.69100717631305031 ) ) ;
#1027 =( BOUNDED_CURVE ( )  B_SPLINE_CURVE ( 2, ( #17419, #3613, #12020, #14762, #14674, #2255, #882, #9215, #13397 ),
 .UNSPECIFIED., .F., .T. ) 
 B_SPLINE_CURVE_WITH_KNOTS ( ( 3, 2, 2, 2, 3 ),
 ( 0.1730769230769231004, 0.1794871794871794879, 0.1923076923076923184, 0.2051282051282051211, 0.2115384615384615641 ),
 .UNSPECIFIED. ) 
 CURVE ( )  GEOMETRIC_REPRESENTATION_ITEM ( )  RATIONAL_B_SPLINE_CURVE ( ( 0.9330127018922194093, 0.9330127018922196314, 1.000000000000000000, 0.8660254037844387076, 1.000000000000000000, 0.8660254037844387076, 1.000000000000000000, 0.9330127018922190762, 0.9330127018922194093 ) ) 
 REPRESENTATION_ITEM ( '' )  );
#1028 = DIRECTION ( 'NONE',  ( 1.000000000000000000, 0.000000000000000000, -0.000000000000000000 ) ) ;
#1029 = CARTESIAN_POINT ( 'NONE',  ( 32.79901970863393501, -6.593096864778464017, -5.783357778048668685 ) ) ;
#1030 = FACE_OUTER_BOUND ( 'NONE', #16056, .T. ) ;
#1031 = AXIS2_PLACEMENT_3D ( 'NONE', #16648, #6847, #5565 ) ;
#1032 = DIRECTION ( 'NONE',  ( 0.9928203230275512992, 0.1196152422706614898, -0.000000000000000000 ) ) ;
#1033 = B_SPLINE_CURVE_WITH_KNOTS ( 'NONE', 3,
 ( #3064, #12661, #14211, #17229, #11661, #4768, #11469, #7150 ),
 .UNSPECIFIED., .F., .F.,
 ( 4, 2, 2, 4 ),
 ( 1.451928974504550231E-19, 0.002450665683189817961, 0.003675998524784728459, 0.004901331366379638524 ),
 .UNSPECIFIED. ) ;
#1034 = VERTEX_POINT ( 'NONE', #3000 ) ;
#1035 = CARTESIAN_POINT ( 'NONE',  ( 25.79194807336802597, -3.038360733637183397, 4.591826007371929919 ) ) ;
#1036 = CARTESIAN_POINT ( 'NONE',  ( 13.65694651542703397, -25.37101204406936361, 16.45580752066269881 ) ) ;
#1037 = CARTESIAN_POINT ( 'NONE',  ( -2.540000000000001368, 3.110602869834278640E-16, 1.599999999999998979 ) ) ;
#1038 = EDGE_CURVE ( 'NONE', #4277, #15625, #10962, .T. ) ;
#1039 = CARTESIAN_POINT ( 'NONE',  ( 32.32036211097666012, -1.624804527518282748, -5.783357778048663356 ) ) ;
#1040 = CARTESIAN_POINT ( 'NONE',  ( 27.46709037723411839, -6.908327297984874882, -4.533357778048668685 ) ) ;
#1041 = DIRECTION ( 'NONE',  ( 1.000000000000000000, 0.000000000000000000, 0.000000000000000000 ) ) ;
#1042 = CARTESIAN_POINT ( 'NONE',  ( -35.74085044863416272, -18.73429073671335132, 11.27079897466147607 ) ) ;
#1043 = DIRECTION ( 'NONE',  ( 0.000000000000000000, 0.000000000000000000, -1.000000000000000000 ) ) ;
#1044 = CARTESIAN_POINT ( 'NONE',  ( 29.14753769709988518, -3.271205139184214516, -3.627061608673662008 ) ) ;
#1045 = LINE ( 'NONE', #10800, #205 ) ;
#1046 = CARTESIAN_POINT ( 'NONE',  ( 32.53688598753899441, -6.297517047505613697, 4.533357778048659803 ) ) ;
#1047 = ORIENTED_EDGE ( 'NONE', *, *, #5609, .T. ) ;
#1048 = PRODUCT_DEFINITION ( 'UNKNOWN', '', #788, #12463 ) ;
#1049 = ORIENTED_EDGE ( 'NONE', *, *, #11408, .F. ) ;
#1050 = CARTESIAN_POINT ( 'NONE',  ( 29.56783163384821833, -3.220568019956291383, 3.627061608673666893 ) ) ;
#1051 = DIRECTION ( 'NONE',  ( 0.000000000000000000, 0.000000000000000000, -1.000000000000000000 ) ) ;
#1052 = CARTESIAN_POINT ( 'NONE',  ( 24.43282520912215006, -22.30499949230690504, 14.60822674442184699 ) ) ;
#1053 = ORIENTED_EDGE ( 'NONE', *, *, #7902, .T. ) ;
#1054 =( NAMED_UNIT ( * ) SI_UNIT ( $, .STERADIAN. ) SOLID_ANGLE_UNIT ( ) );
#1055 = FACE_OUTER_BOUND ( 'NONE', #13406, .T. ) ;
#1056 = EDGE_CURVE ( 'NONE', #13311, #2108, #11302, .T. ) ;
#1057 = CARTESIAN_POINT ( 'NONE',  ( 28.04870365451522218, -4.657534006690712935, -8.283357778048662468 ) ) ;
#1058 = CARTESIAN_POINT ( 'NONE',  ( 30.30787278169304244, -6.266260340387784566, -4.705209693361169343 ) ) ;
#1059 = CYLINDRICAL_SURFACE ( 'NONE', #5164, 5.500000000000000888 ) ;
#1060 = CARTESIAN_POINT ( 'NONE',  ( -10.50000000000000000, 0.000000000000000000, -2.000000000000000000 ) ) ;
#1061 = CARTESIAN_POINT ( 'NONE',  ( 26.97161122272022382, -2.906390775372597712, 6.861505862736165362 ) ) ;
#1062 = DIRECTION ( 'NONE',  ( -0.000000000000000000, -0.000000000000000000, 1.000000000000000000 ) ) ;
#1063 = CARTESIAN_POINT ( 'NONE',  ( 0.000000000000000000, 0.000000000000000000, -10.50000000000000000 ) ) ;
#1064 = ADVANCED_FACE ( 'NONE', ( #3085 ), #7359, .F. ) ;
#1065 = CARTESIAN_POINT ( 'NONE',  ( 0.000000000000000000, 0.000000000000000000, 0.000000000000000000 ) ) ;
#1066 = CARTESIAN_POINT ( 'NONE',  ( 29.46348657678868577, -6.667800981652280967, 4.533357778048659803 ) ) ;
#1067 = ORIENTED_EDGE ( 'NONE', *, *, #5837, .F. ) ;
#1068 = ORIENTED_EDGE ( 'NONE', *, *, #3042, .T. ) ;
#1069 = VERTEX_POINT ( 'NONE', #8885 ) ;
#1070 = CARTESIAN_POINT ( 'NONE',  ( 32.14665875496697822, -6.044722943765660439, 4.705209693361160461 ) ) ;
#1071 = DIRECTION ( 'NONE',  ( 0.9928203230275512992, 0.1196152422706610041, 9.614813431917824012E-17 ) ) ;
#1072 = CARTESIAN_POINT ( 'NONE',  ( 30.39102621733566423, -5.629271460726127607, 3.627061608673662896 ) ) ;
#1073 = ORIENTED_EDGE ( 'NONE', *, *, #2262, .F. ) ;
#1074 = FACE_OUTER_BOUND ( 'NONE', #8041, .T. ) ;
#1075 = LINE ( 'NONE', #6598, #7885 ) ;
#1076 = CARTESIAN_POINT ( 'NONE',  ( 31.04338717100262102, -6.177645381738930297, -6.861505862736167138 ) ) ;
#1077 = CARTESIAN_POINT ( 'NONE',  ( 28.50956232500783472, -2.083930644370540985, -6.453230759126464378 ) ) ;
#1079 = EDGE_CURVE ( 'NONE', #5626, #14839, #12411, .T. ) ;
#1078 = CARTESIAN_POINT ( 'NONE',  ( 31.83134908525019213, -4.201799933639492224, -8.283357778048662468 ) ) ;
#1080 = CARTESIAN_POINT ( 'NONE',  ( 31.71123609653335507, -2.762457591843783256, 3.283357778048666464 ) ) ;
#1081 = CARTESIAN_POINT ( 'NONE',  ( 27.86926259684567597, -5.933094176093606897, -7.939653947423664704 ) ) ;
#1082 = CARTESIAN_POINT ( 'NONE',  ( 29.71979337562451207, -1.938121702948446323, -5.783357778048664244 ) ) ;
#1083 = CARTESIAN_POINT ( 'NONE',  ( 30.80679339554874119, -2.444327062417882779, -6.861505862736158257 ) ) ;
#1084 = EDGE_CURVE ( 'NONE', #9477, #14231, #5339, .T. ) ;
#1085 = CARTESIAN_POINT ( 'NONE',  ( 32.93018312783485868, -2.815471066132993805, -3.627061608673662008 ) ) ;
#1086 = ORIENTED_EDGE ( 'NONE', *, *, #10347, .F. ) ;
#1087 = EDGE_CURVE ( 'NONE', #17201, #15670, #17322, .T. ) ;
#1088 = CARTESIAN_POINT ( 'NONE',  ( 30.42903939560917337, -1.852671564043892660, -5.783357778048658027 ) ) ;
#1089 = CARTESIAN_POINT ( 'NONE',  ( -2.016448651773435938E-27, -20.49999999999999645, -17.00000000000000000 ) ) ;
#1090 =( BOUNDED_CURVE ( )  B_SPLINE_CURVE ( 2, ( #14792, #14707, #2289, #10422, #918, #9082, #10592, #14623, #11605 ),
 .UNSPECIFIED., .F., .T. ) 
 B_SPLINE_CURVE_WITH_KNOTS ( ( 3, 2, 2, 2, 3 ),
 ( 0.05769230769230770939, 0.06410256410256409687, 0.07692307692307692735, 0.08974358974358974395, 0.09615384615384617306 ),
 .UNSPECIFIED. ) 
 CURVE ( )  GEOMETRIC_REPRESENTATION_ITEM ( )  RATIONAL_B_SPLINE_CURVE ( ( 0.9330127018922194093, 0.9330127018922196314, 1.000000000000000000, 0.8660254037844387076, 1.000000000000000000, 0.8660254037844387076, 1.000000000000000000, 0.9330127018922191873, 0.9330127018922194093 ) ) 
 REPRESENTATION_ITEM ( '' )  );
#1091 = CIRCLE ( 'NONE', #3704, 2.000000000000001776 ) ;
#1092 = ORIENTED_EDGE ( 'NONE', *, *, #6411, .F. ) ;
#1093 = CARTESIAN_POINT ( 'NONE',  ( 31.30154412293507349, -3.011689903141150815, 3.627061608673666449 ) ) ;
#1094 = CARTESIAN_POINT ( 'NONE',  ( 27.75549246765397271, -7.200742295513424374, -5.783357778048668685 ) ) ;
#1095 = CARTESIAN_POINT ( 'NONE',  ( 28.04870365451522218, -4.657534006690712935, 3.283357778048664244 ) ) ;
#1096 = PLANE ( 'NONE',  #10161 ) ;
#1097 = DIRECTION ( 'NONE',  ( 1.000000000000000000, 0.000000000000000000, 0.000000000000000000 ) ) ;
#1098 = EDGE_CURVE ( 'NONE', #15002, #2720, #10409, .T. ) ;
#1099 = DIRECTION ( 'NONE',  ( -0.000000000000000000, -0.000000000000000000, 1.000000000000000000 ) ) ;
#1100 = CARTESIAN_POINT ( 'NONE',  ( 30.67935139548315604, -7.248220074880824981, -5.783357778048669573 ) ) ;
#1101 = CIRCLE ( 'NONE', #12980, 2.749999999999988454 ) ;
#1102 = ORIENTED_EDGE ( 'NONE', *, *, #11417, .F. ) ;
#1103 = CARTESIAN_POINT ( 'NONE',  ( 2.000000000000002220, 3.464101615137753054, -2.842992957459234304 ) ) ;
#1104 = EDGE_CURVE ( 'NONE', #17832, #13470, #5059, .T. ) ;
#1105 = DIRECTION ( 'NONE',  ( 0.9928203230275510771, 0.1196152422706609902, 4.006172263299092517E-17 ) ) ;
#1106 = CARTESIAN_POINT ( 'NONE',  ( 1.828356344711638881, 3.563200125723181344, -1.227350740571481191E-15 ) ) ;
#1107 = DIRECTION ( 'NONE',  ( -1.000000000000000000, 0.000000000000000000, 0.000000000000000000 ) ) ;
#1108 = CARTESIAN_POINT ( 'NONE',  ( -0.5449245075114568237, -4.304189842417255996, -3.016622336522495118 ) ) ;
#1109 = CARTESIAN_POINT ( 'NONE',  ( 31.39792096211754924, -4.254019462947003838, -7.939653947423662039 ) ) ;
#1110 =( BOUNDED_CURVE ( )  B_SPLINE_CURVE ( 2, ( #15566, #14564, #348, #6199, #6287, #14645, #7660, #11809, #13269 ),
 .UNSPECIFIED., .F., .T. ) 
 B_SPLINE_CURVE_WITH_KNOTS ( ( 3, 2, 2, 2, 3 ),
 ( 0.2884615384615384914, 0.2948717948717948789, 0.3076923076923077094, 0.3205128205128205399, 0.3269230769230769273 ),
 .UNSPECIFIED. ) 
 CURVE ( )  GEOMETRIC_REPRESENTATION_ITEM ( )  RATIONAL_B_SPLINE_CURVE ( ( 0.9330127018922194093, 0.9330127018922196314, 1.000000000000000000, 0.8660254037844387076, 1.000000000000000000, 0.8660254037844387076, 1.000000000000000000, 0.9330127018922194093, 0.9330127018922194093 ) ) 
 REPRESENTATION_ITEM ( '' )  );
#1111 = ADVANCED_FACE ( 'NONE', ( #3631 ), #15964, .F. ) ;
#1112 = ORIENTED_EDGE ( 'NONE', *, *, #278, .T. ) ;
#1113 = CIRCLE ( 'NONE', #16478, 13.60000000000000320 ) ;
#1114 = ORIENTED_EDGE ( 'NONE', *, *, #13801, .T. ) ;
#1115 = DIRECTION ( 'NONE',  ( -0.1196152422706611984, 0.9928203230275510771, 0.000000000000000000 ) ) ;
#1116 = CIRCLE ( 'NONE', #14443, 6.249999999999996447 ) ;
#1117 = ORIENTED_EDGE ( 'NONE', *, *, #17232, .F. ) ;
#1118 = APPLICATION_CONTEXT ( 'automotive_design' ) ;
#1119 = FILL_AREA_STYLE ('',( #13542 ) ) ;
#1120 = CARTESIAN_POINT ( 'NONE',  ( 32.81641299864316608, -4.083119185552795294, -7.939653947423662039 ) ) ;
#1121 = CARTESIAN_POINT ( 'NONE',  ( 25.11802603177690330, -16.03270077640482683, 0.5379818257722508434 ) ) ;
#1122 = CARTESIAN_POINT ( 'NONE',  ( 27.10304229683147526, -4.771467524953526329, -3.283357778048664688 ) ) ;
#1123 = FACE_BOUND ( 'NONE', #12437, .T. ) ;
#1124 = CARTESIAN_POINT ( 'NONE',  ( 0.000000000000000000, 0.000000000000000000, -4.674599999999997202 ) ) ;
#1125 = CARTESIAN_POINT ( 'NONE',  ( 27.78610916120306129, -6.570083055755264745, -4.705209693361169343 ) ) ;
#1126 = CARTESIAN_POINT ( 'NONE',  ( 0.000000000000000000, 0.000000000000000000, -4.674599999999997202 ) ) ;
#1127 = CARTESIAN_POINT ( 'NONE',  ( 31.24221605398236790, -5.726592414339752857, 3.283357778048663800 ) ) ;
#1128 = EDGE_LOOP ( 'NONE', ( #16946, #361, #10128, #4367 ) ) ;
#1129 = EDGE_CURVE ( 'NONE', #4586, #7873, #17252, .T. ) ;
#1130 = CARTESIAN_POINT ( 'NONE',  ( 29.78250536075762867, -6.329556739422670830, 4.705209693361159573 ) ) ;
#1131 = DIRECTION ( 'NONE',  ( -0.5999999999999999778, 0.7999999999999999334, -0.000000000000000000 ) ) ;
#1132 = CARTESIAN_POINT ( 'NONE',  ( 24.62797819841904001, -22.25577170577939157, 14.56336204217505426 ) ) ;
#1133 = ORIENTED_EDGE ( 'NONE', *, *, #3776, .F. ) ;
#1134 = PRESENTATION_STYLE_ASSIGNMENT (( #9546 ) ) ;
#1135 = EDGE_LOOP ( 'NONE', ( #15094, #7609 ) ) ;
#1136 = AXIS2_PLACEMENT_3D ( 'NONE', #7243, #8688, #3068 ) ;
#1137 = CARTESIAN_POINT ( 'NONE',  ( 13.00000000000000178, 0.000000000000000000, -6.000000000000000000 ) ) ;
#1138 = EDGE_CURVE ( 'NONE', #9324, #12386, #9302, .T. ) ;
#1139 = EDGE_LOOP ( 'NONE', ( #14257, #12890, #1424, #3754, #13267, #12091 ) ) ;
#1140 = CARTESIAN_POINT ( 'NONE',  ( 32.87199790123699472, -1.558343308739095656, -5.783357778048663356 ) ) ;
#1141 = EDGE_CURVE ( 'NONE', #11286, #5484, #11940, .T. ) ;
#1142 = CARTESIAN_POINT ( 'NONE',  ( 29.14753769709988518, -3.271205139184214516, -3.627061608673662008 ) ) ;
#1143 = ORIENTED_EDGE ( 'NONE', *, *, #6595, .F. ) ;
#1144 = CARTESIAN_POINT ( 'NONE',  ( -4.175647895129166898, 2.207990717223085930, -3.169390900447850878 ) ) ;
#1145 = DIRECTION ( 'NONE',  ( -0.000000000000000000, -0.000000000000000000, 1.000000000000000000 ) ) ;
#1146 = DIRECTION ( 'NONE',  ( 5.026720092345836698E-22, -4.581671729415424240E-22, 1.000000000000000000 ) ) ;
#1147 = CARTESIAN_POINT ( 'NONE',  ( 32.55182397003001427, -2.661183353387966299, 8.283357778048666020 ) ) ;
#1148 = VECTOR ( 'NONE', #6040, 1000.000000000000000 ) ;
#1149 = AXIS2_PLACEMENT_3D ( 'NONE', #5454, #8274, #1391 ) ;
#1150 = PRODUCT_DEFINITION_SHAPE ( 'NONE', 'NONE',  #17976 ) ;
#1151 = CARTESIAN_POINT ( 'NONE',  ( 29.82181869931131146, -4.443908660051686610, 7.939653947423662039 ) ) ;
#1152 = CARTESIAN_POINT ( 'NONE',  ( 11.73134587110777005, 4.864722402403120149, -9.600000000000001421 ) ) ;
#1153 = CARTESIAN_POINT ( 'NONE',  ( 0.000000000000000000, 0.000000000000000000, 10.50000000000000000 ) ) ;
#1154 = CARTESIAN_POINT ( 'NONE',  ( 32.08959525433819238, -2.916745304588811649, 3.627061608673666893 ) ) ;
#1155 = CARTESIAN_POINT ( 'NONE',  ( 27.89480254248674740, -2.495355674045408367, 4.533357778048667797 ) ) ;
#1156 = VECTOR ( 'NONE', #15774, 1000.000000000000227 ) ;
#1157 = ADVANCED_FACE ( 'NONE', ( #14513 ), #7792, .T. ) ;
#1158 = VERTEX_POINT ( 'NONE', #9063 ) ;
#1159 = EDGE_CURVE ( 'NONE', #13209, #11980, #1304, .T. ) ;
#1160 = ORIENTED_EDGE ( 'NONE', *, *, #5892, .T. ) ;
#1161 = VERTEX_POINT ( 'NONE', #7972 ) ;
#1162 = CARTESIAN_POINT ( 'NONE',  ( 33.17547354829333273, -5.293800545841212291, 7.939653947423658487 ) ) ;
#1163 = CARTESIAN_POINT ( 'NONE',  ( 28.83304567166618781, -6.743756660494150346, -7.033357778048666908 ) ) ;
#1164 = CARTESIAN_POINT ( 'NONE',  ( 29.67743187657054449, -6.342216019229654833, 6.861505862736157368 ) ) ;
#1165 = ORIENTED_EDGE ( 'NONE', *, *, #5934, .F. ) ;
#1166 = CARTESIAN_POINT ( 'NONE',  ( 29.89119874204131122, -2.254829357712824667, 7.033357778048666020 ) ) ;
#1167 = DIRECTION ( 'NONE',  ( 0.9928203230275510771, 0.1196152422706609902, 4.006172263299092517E-17 ) ) ;
#1168 = CARTESIAN_POINT ( 'NONE',  ( 29.39961944441754227, -3.040961747597316744, -3.283357778048662023 ) ) ;
#1169 = CARTESIAN_POINT ( 'NONE',  ( -34.91600907648203389, -11.88801210197604341, 11.56671555609732671 ) ) ;
#1170 = CARTESIAN_POINT ( 'NONE',  ( 26.20438954464326287, -6.461672570559207074, -7.734911333299593572 ) ) ;
#1171 = EDGE_LOOP ( 'NONE', ( #9781, #9162 ) ) ;
#1172 = AXIS2_PLACEMENT_3D ( 'NONE', #8228, #13759, #1339 ) ;
#1173 = CARTESIAN_POINT ( 'NONE',  ( 31.95146207396702565, -5.641142275435198528, -8.283357778048662468 ) ) ;
#1174 = CYLINDRICAL_SURFACE ( 'NONE', #14258, 2.500000000000001776 ) ;
#1175 = CARTESIAN_POINT ( 'NONE',  ( 23.43390247958827288, -9.970148115950962620, -14.83177094038517652 ) ) ;
#1176 = CARTESIAN_POINT ( 'NONE',  ( 26.04410741498555382, -2.380969272135942560, 6.453230759126468818 ) ) ;
#1177 = SURFACE_SIDE_STYLE ('',( #3895 ) ) ;
#1178 = CARTESIAN_POINT ( 'NONE',  ( 33.13163345120441505, -4.045141346131868154, -3.627061608673664672 ) ) ;
#1179 = VECTOR ( 'NONE', #10787, 1000.000000000000114 ) ;
#1180 = CARTESIAN_POINT ( 'NONE',  ( 30.18087924896149588, -5.654590020340094725, -3.627061608673668225 ) ) ;
#1181 = AXIS2_PLACEMENT_3D ( 'NONE', #7932, #13466, #1041 ) ;
#1182 = CARTESIAN_POINT ( 'NONE',  ( 5.200000000000002842, 0.000000000000000000, 0.000000000000000000 ) ) ;
#1183 = DIRECTION ( 'NONE',  ( 0.1196152422706587976, -0.9928203230275515212, 1.866876274697368064E-15 ) ) ;
#1184 = VERTEX_POINT ( 'NONE', #9571 ) ;
#1185 = CIRCLE ( 'NONE', #14801, 2.749999999999991118 ) ;
#1186 = EDGE_CURVE ( 'NONE', #63, #14701, #1906, .T. ) ;
#1187 = EDGE_LOOP ( 'NONE', ( #16383, #1379, #6856, #3698 ) ) ;
#1188 = CARTESIAN_POINT ( 'NONE',  ( 30.65370992780335868, -5.597623261208692469, 7.939653947423658487 ) ) ;
#1189 = CARTESIAN_POINT ( 'NONE',  ( 28.14933959732260149, -3.391468297350500372, -7.939653947423660263 ) ) ;
#1190 = LINE ( 'NONE', #7567, #15018 ) ;
#1191 = CARTESIAN_POINT ( 'NONE',  ( -45.50000000000000000, -16.03270077640482683, -8.287981825772238409 ) ) ;
#1192 = AXIS2_PLACEMENT_3D ( 'NONE', #16349, #13436, #5076 ) ;
#1193 = CARTESIAN_POINT ( 'NONE',  ( 32.30788887834420819, -1.963665922152317833, 4.533357778048667797 ) ) ;
#1194 = EDGE_CURVE ( 'NONE', #17090, #11418, #15122, .T. ) ;
#1195 = DIRECTION ( 'NONE',  ( 0.000000000000000000, 0.000000000000000000, 1.000000000000000000 ) ) ;
#1196 = CARTESIAN_POINT ( 'NONE',  ( 29.07687923786957285, -2.352938776424351008, -7.033357778048658027 ) ) ;
#1197 = VECTOR ( 'NONE', #9155, 1000.000000000000000 ) ;
#1198 = VERTEX_POINT ( 'NONE', #8051 ) ;
#1199 = CARTESIAN_POINT ( 'NONE',  ( 0.000000000000000000, 0.000000000000000000, -4.000000000000000000 ) ) ;
#1200 = CARTESIAN_POINT ( 'NONE',  ( 28.53771668024168662, -2.080538600569502794, 5.783357778048667797 ) ) ;
#1201 = CARTESIAN_POINT ( 'NONE',  ( 30.49166216014303643, -4.363205751385915931, -8.283357778048662468 ) ) ;
#1202 = CARTESIAN_POINT ( 'NONE',  ( 27.90727577511918867, -2.156494279411373061, -5.783357778048670461 ) ) ;
#1203 =( BOUNDED_CURVE ( )  B_SPLINE_CURVE ( 2, ( #13490, #8126, #10907, #3786, #6418, #7870, #10825, #15012, #6769 ),
 .UNSPECIFIED., .F., .T. ) 
 B_SPLINE_CURVE_WITH_KNOTS ( ( 3, 2, 2, 2, 3 ),
 ( 0.6730769230769231282, 0.6794871794871795156, 0.6923076923076922906, 0.7051282051282051766, 0.7115384615384615641 ),
 .UNSPECIFIED. ) 
 CURVE ( )  GEOMETRIC_REPRESENTATION_ITEM ( )  RATIONAL_B_SPLINE_CURVE ( ( 0.9330127018922192983, 0.9330127018922198534, 1.000000000000000000, 0.8660254037844387076, 1.000000000000000000, 0.8660254037844387076, 1.000000000000000000, 0.9330127018922194093, 0.9330127018922194093 ) ) 
 REPRESENTATION_ITEM ( '' )  );
#1204 = CARTESIAN_POINT ( 'NONE',  ( -29.25000000000000000, -16.21813761408365195, 13.00000000000000178 ) ) ;
#1205 = CARTESIAN_POINT ( 'NONE',  ( 30.12381574833269937, -2.526612381163247267, -4.705209693361161349 ) ) ;
#1206 = VECTOR ( 'NONE', #4523, 1000.000000000000227 ) ;
#1207 = AXIS2_PLACEMENT_3D ( 'NONE', #15325, #4498, #15560 ) ;
#1208 = ADVANCED_FACE ( 'NONE', ( #1342 ), #12312, .T. ) ;
#1209 = AXIS2_PLACEMENT_3D ( 'NONE', #2238, #17500, #17400 ) ;
#1210 = LINE ( 'NONE', #15070, #3594 ) ;
#1211 = AXIS2_PLACEMENT_3D ( 'NONE', #12487, #8755, #7400 ) ;
#1212 = ORIENTED_EDGE ( 'NONE', *, *, #11508, .T. ) ;
#1213 = DIRECTION ( 'NONE',  ( 1.000000000000000000, 0.000000000000000000, 0.000000000000000000 ) ) ;
#1214 = ORIENTED_EDGE ( 'NONE', *, *, #5761, .F. ) ;
#1215 = CARTESIAN_POINT ( 'NONE',  ( 25.84832697747032526, -3.506312147857045147, 3.985547620975729899 ) ) ;
#1216 = EDGE_CURVE ( 'NONE', #14120, #8870, #2004, .T. ) ;
#1217 = CARTESIAN_POINT ( 'NONE',  ( 29.15206445563513071, -6.405512418264540209, -6.861505862736167138 ) ) ;
#1218 = DIRECTION ( 'NONE',  ( 0.9928203230275511881, 0.1196152422706614898, 0.000000000000000000 ) ) ;
#1219 = AXIS2_PLACEMENT_3D ( 'NONE', #3482, #3148, #675 ) ;
#1220 = CIRCLE ( 'NONE', #12162, 25.00000000000000000 ) ;
#1221 = CARTESIAN_POINT ( 'NONE',  ( 26.00347982711925710, -2.723222710571018279, -7.033357778048658027 ) ) ;
#1222 = PLANE ( 'NONE',  #13590 ) ;
#1223 = AXIS2_PLACEMENT_3D ( 'NONE', #1707, #3242, #10293 ) ;
#1224 = CYLINDRICAL_SURFACE ( 'NONE', #802, 2.500000000000000888 ) ;
#1225 = VECTOR ( 'NONE', #2570, 1000.000000000000000 ) ;
#1226 = CARTESIAN_POINT ( 'NONE',  ( 25.88156304229571703, -4.918631652813365562, -7.939653947423662039 ) ) ;
#1227 = AXIS2_PLACEMENT_3D ( 'NONE', #5967, #9955, #14335 ) ;
#1228 = ORIENTED_EDGE ( 'NONE', *, *, #11996, .F. ) ;
#1229 = CARTESIAN_POINT ( 'NONE',  ( 28.74176732417158320, -7.092112515190875044, 5.783357778048669573 ) ) ;
#1230 = CARTESIAN_POINT ( 'NONE',  ( 31.02146712245815507, -5.553315781884258229, 3.627061608673662896 ) ) ;
#1231 = CARTESIAN_POINT ( 'NONE',  ( 34.91600907648203389, -11.88801210197604341, 0.000000000000000000 ) ) ;
#1232 = CARTESIAN_POINT ( 'NONE',  ( 18.90799107099199716, -20.96007437013451380, 15.70102267215298042 ) ) ;
#1233 = ORIENTED_EDGE ( 'NONE', *, *, #16362, .F. ) ;
#1234 = CARTESIAN_POINT ( 'NONE',  ( 31.61111609099199171, -1.710254666422835745, -5.783357778048661579 ) ) ;
#1235 = CIRCLE ( 'NONE', #11336, 2.500000000000000000 ) ;
#1236 = VERTEX_POINT ( 'NONE', #10842 ) ;
#1237 = DIRECTION ( 'NONE',  ( 0.000000000000000000, 0.000000000000000000, -1.000000000000000000 ) ) ;
#1238 = CARTESIAN_POINT ( 'NONE',  ( 9.099998387031005720, -19.29508120620799971, -16.81964500401478091 ) ) ;
#1239 = CARTESIAN_POINT ( 'NONE',  ( 29.34898802046944155, -4.500875419183088866, -3.627061608673664672 ) ) ;
#1240 = ADVANCED_FACE ( 'NONE', ( #2709 ), #17880, .T. ) ;
#1241 = DIRECTION ( 'NONE',  ( -0.8243186046180107640, -0.5661261679878573094, 0.000000000000000000 ) ) ;
#1242 = CIRCLE ( 'NONE', #15137, 2.749999999999991118 ) ;
#1243 = DIRECTION ( 'NONE',  ( 0.000000000000000000, 0.000000000000000000, -1.000000000000000000 ) ) ;
#1244 = DIRECTION ( 'NONE',  ( 1.000000000000000000, 0.000000000000000000, 0.000000000000000000 ) ) ;
#1245 = LINE ( 'NONE', #16555, #5173 ) ;
#1246 = CARTESIAN_POINT ( 'NONE',  ( 28.12741954877813555, -2.767138697495831856, 4.705209693361167567 ) ) ;
#1247 = AXIS2_PLACEMENT_3D ( 'NONE', #8112, #9206, #12096 ) ;
#1248 = DIRECTION ( 'NONE',  ( 0.000000000000000000, 0.4999999999999992784, -0.8660254037844390407 ) ) ;
#1249 = CARTESIAN_POINT ( 'NONE',  ( -3.538288549924106796, -15.34800872113743431, -13.00000000000000178 ) ) ;
#1250 = CARTESIAN_POINT ( 'NONE',  ( 33.56515079149260572, -5.873822666371450119, 4.705209693361159573 ) ) ;
#1251 = AXIS2_PLACEMENT_3D ( 'NONE', #8210, #8025, #13562 ) ;
#1252 = EDGE_CURVE ( 'NONE', #2160, #254, #5493, .T. ) ;
#1253 = ADVANCED_FACE ( 'NONE', ( #5403 ), #4162, .T. ) ;
#1254 = ORIENTED_EDGE ( 'NONE', *, *, #12502, .T. ) ;
#1255 = ORIENTED_EDGE ( 'NONE', *, *, #3739, .F. ) ;
#1256 = CARTESIAN_POINT ( 'NONE',  ( 33.17094678975809074, -2.159493266760871499, 4.705209693361167567 ) ) ;
#1257 = CIRCLE ( 'NONE', #6474, 0.9999999999999995559 ) ;
#1258 = DIRECTION ( 'NONE',  ( -0.8660254037844397068, -0.4999999999999981126, 0.000000000000000000 ) ) ;
#1259 = VERTEX_POINT ( 'NONE', #14780 ) ;
#1260 = CARTESIAN_POINT ( 'NONE',  ( 29.13014440709066832, -5.781182818409868140, 3.627061608673662896 ) ) ;
#1261 = DIRECTION ( 'NONE',  ( 0.000000000000000000, 0.000000000000000000, 1.000000000000000000 ) ) ;
#1262 = DIRECTION ( 'NONE',  ( -0.1196152422706610735, 0.9928203230275511881, 0.000000000000000000 ) ) ;
#1263 = CARTESIAN_POINT ( 'NONE',  ( 8.632250723006720250, -18.84644399697197770, 13.00000000000000178 ) ) ;
#1264 = VECTOR ( 'NONE', #15862, 1000.000000000000000 ) ;
#1265 = DIRECTION ( 'NONE',  ( -1.000000000000000000, 0.000000000000000000, 0.000000000000000000 ) ) ;
#1266 = CARTESIAN_POINT ( 'NONE',  ( 28.04870365451522218, -4.657534006690712935, -8.283357778048662468 ) ) ;
#1267 = CARTESIAN_POINT ( 'NONE',  ( 31.97277696464621854, -6.702839660918840536, 5.783357778048664244 ) ) ;
#1268 = EDGE_CURVE ( 'NONE', #4798, #16432, #724, .T. ) ;
#1269 = CARTESIAN_POINT ( 'NONE',  ( 27.95350797341489368, -12.38528642892598342, -13.73189064827997541 ) ) ;
#1270 = CARTESIAN_POINT ( 'NONE',  ( 26.10855331130634127, -2.710563430764044490, 7.033357778048666020 ) ) ;
#1271 = SURFACE_STYLE_USAGE ( .BOTH. , #17804 ) ;
#1272 = CARTESIAN_POINT ( 'NONE',  ( 32.82963640218302004, -5.962437625020304388, -4.705209693361169343 ) ) ;
#1273 = CARTESIAN_POINT ( 'NONE',  ( 27.65911562847151117, -5.958412735707574015, -3.627061608673668225 ) ) ;
#1274 = VERTEX_POINT ( 'NONE', #13589 ) ;
#1275 = CARTESIAN_POINT ( 'NONE',  ( 31.51612863268893960, -4.239777773060436239, 8.283357778048662468 ) ) ;
#1276 = CARTESIAN_POINT ( 'NONE',  ( 33.60446413004628141, -3.988174587000466342, -3.627061608673664672 ) ) ;
#1277 = ORIENTED_EDGE ( 'NONE', *, *, #12144, .F. ) ;
#1278 = CARTESIAN_POINT ( 'NONE',  ( 33.28924367748503244, -4.026152426421394814, 3.627061608673664228 ) ) ;
#1279 = CARTESIAN_POINT ( 'NONE',  ( 28.34209327568754944, -5.876127416962207306, -7.939653947423662927 ) ) ;
#1280 = CARTESIAN_POINT ( 'NONE',  ( 25.80685721358263152, -3.162108319002908896, -4.519686641326834398 ) ) ;
#1281 = DIRECTION ( 'NONE',  ( 0.000000000000000000, 0.000000000000000000, -1.000000000000000000 ) ) ;
#1282 = CARTESIAN_POINT ( 'NONE',  ( 28.87615734162756453, -4.557842178314484016, -7.939653947423662039 ) ) ;
#1283 = CARTESIAN_POINT ( 'NONE',  ( 0.000000000000000000, 0.000000000000000000, 13.31572692736085095 ) ) ;
#1284 = CARTESIAN_POINT ( 'NONE',  ( -5.499998387031001634, -20.49508120620799900, -6.000000000000000000 ) ) ;
#1285 = DIRECTION ( 'NONE',  ( -1.000000000000000000, -0.000000000000000000, -0.000000000000000000 ) ) ;
#1286 = ADVANCED_FACE ( 'NONE', ( #5143 ), #13418, .F. ) ;
#1287 = CARTESIAN_POINT ( 'NONE',  ( 29.32081432955537892, -3.050456207659999475, -3.283357778048662023 ) ) ;
#1288 = EDGE_LOOP ( 'NONE', ( #15134, #15555, #15815, #8257 ) ) ;
#1289 = DIRECTION ( 'NONE',  ( -1.000000000000000000, 0.000000000000000000, 0.000000000000000000 ) ) ;
#1290 = CARTESIAN_POINT ( 'NONE',  ( -1.500000000000000000, -10.39230484541326405, -3.000000000000002665 ) ) ;
#1291 = DIRECTION ( 'NONE',  ( 0.000000000000000000, 0.000000000000000000, -1.000000000000000000 ) ) ;
#1292 = CARTESIAN_POINT ( 'NONE',  ( 26.01652455409633902, -4.902371455920928156, -5.783357778048663356 ) ) ;
#1293 = ORIENTED_EDGE ( 'NONE', *, *, #12859, .F. ) ;
#1294 = CARTESIAN_POINT ( 'NONE',  ( 25.89088658894545603, -2.009881179784104965, -5.783357778048658027 ) ) ;
#1295 = CARTESIAN_POINT ( 'NONE',  ( 28.76238721243587548, -5.825490297734302381, -3.627061608673667781 ) ) ;
#1296 = EDGE_CURVE ( 'NONE', #16733, #3360, #5319, .T. ) ;
#1297 = DIRECTION ( 'NONE',  ( 1.000000000000000000, 0.000000000000000000, 0.000000000000000000 ) ) ;
#1298 = VERTEX_POINT ( 'NONE', #3975 ) ;
#1299 = FACE_OUTER_BOUND ( 'NONE', #12715, .T. ) ;
#1300 = ORIENTED_EDGE ( 'NONE', *, *, #4267, .T. ) ;
#1301 = CARTESIAN_POINT ( 'NONE',  ( 29.13014440709066832, -5.781182818409868140, -7.939653947423662927 ) ) ;
#1302 = ORIENTED_EDGE ( 'NONE', *, *, #3384, .T. ) ;
#1303 = DIRECTION ( 'NONE',  ( -1.000000000000000000, 0.000000000000000000, 0.000000000000000000 ) ) ;
#1304 =( BOUNDED_CURVE ( )  B_SPLINE_CURVE ( 2, ( #722, #9231, #6247, #2188, #13229, #6337, #13322, #17961, #17624 ),
 .UNSPECIFIED., .F., .T. ) 
 B_SPLINE_CURVE_WITH_KNOTS ( ( 3, 2, 2, 2, 3 ),
 ( 0.5576923076923077094, 0.5641025641025640969, 0.5769230769230768718, 0.5897435897435897578, 0.5961538461538461453 ),
 .UNSPECIFIED. ) 
 CURVE ( )  GEOMETRIC_REPRESENTATION_ITEM ( )  RATIONAL_B_SPLINE_CURVE ( ( 0.9330127018922194093, 0.9330127018922194093, 1.000000000000000000, 0.8660254037844387076, 1.000000000000000000, 0.8660254037844387076, 1.000000000000000000, 0.9330127018922194093, 0.9330127018922194093 ) ) 
 REPRESENTATION_ITEM ( '' )  );
#1305 = EDGE_CURVE ( 'NONE', #3946, #4809, #15975, .T. ) ;
#1306 = CARTESIAN_POINT ( 'NONE',  ( 25.63782166807609997, -6.407846580969937200, -7.820349034508990549 ) ) ;
#1307 = DIRECTION ( 'NONE',  ( 0.8660254037844397068, 0.4999999999999981126, -0.000000000000000000 ) ) ;
#1308 = CARTESIAN_POINT ( 'NONE',  ( 0.000000000000000000, 0.000000000000000000, -2.000000000000000000 ) ) ;
#1309 = CARTESIAN_POINT ( 'NONE',  ( 26.39823381822651882, -6.110324093391315436, -3.627061608673668225 ) ) ;
#1310 = DIRECTION ( 'NONE',  ( -0.1196152422706598106, 0.9928203230275514102, 0.000000000000000000 ) ) ;
#1311 = EDGE_CURVE ( 'NONE', #15079, #1236, #3214, .T. ) ;
#1312 = CARTESIAN_POINT ( 'NONE',  ( 25.96861057204955259, -6.167300557297518360, 4.026422103237231376 ) ) ;
#1313 = CARTESIAN_POINT ( 'NONE',  ( -17.40654580017221065, -13.42197210625884551, 15.93919332483364748 ) ) ;
#1314 = CARTESIAN_POINT ( 'NONE',  ( -4.204015924366189871, 1.626724848190924444, -3.310627190413392817 ) ) ;
#1315 = ORIENTED_EDGE ( 'NONE', *, *, #13930, .F. ) ;
#1316 = CARTESIAN_POINT ( 'NONE',  ( 32.46178999037268653, -4.125844254797621957, -8.283357778048662468 ) ) ;
#1317 = EDGE_LOOP ( 'NONE', ( #16339, #11212, #14885, #12801, #7636 ) ) ;
#1318 = DIRECTION ( 'NONE',  ( 0.9396926207859104263, 0.000000000000000000, 0.3420201433256631063 ) ) ;
#1319 = VERTEX_POINT ( 'NONE', #11722 ) ;
#1320 = CARTESIAN_POINT ( 'NONE',  ( 30.80679339554874119, -2.444327062417882779, -6.861505862736158257 ) ) ;
#1321 = EDGE_CURVE ( 'NONE', #14985, #12543, #4242, .T. ) ;
#1322 = DIRECTION ( 'NONE',  ( 1.000000000000000000, 0.000000000000000000, 0.000000000000000000 ) ) ;
#1323 = CARTESIAN_POINT ( 'NONE',  ( 27.96989853965305528, -4.667028466753395222, 3.283357778048664244 ) ) ;
#1324 = CARTESIAN_POINT ( 'NONE',  ( -2.016448651773435938E-27, -20.49999999999999645, -18.00000000000000711 ) ) ;
#1325 = CARTESIAN_POINT ( 'NONE',  ( 27.10313151398701947, -6.652368374500619908, 4.705209693361160461 ) ) ;
#1326 = CARTESIAN_POINT ( 'NONE',  ( 27.73357241910951743, -6.576412695658750529, 4.705209693361160461 ) ) ;
#1327 = DIRECTION ( 'NONE',  ( 0.9928203230275510771, 0.1196152422706614621, -0.000000000000000000 ) ) ;
#1328 = CARTESIAN_POINT ( 'NONE',  ( 26.24741491880506672, -3.420740141806666301, -3.283357778048662023 ) ) ;
#1329 = CARTESIAN_POINT ( 'NONE',  ( 33.30663696749426350, -1.516174747195733863, 5.783357778048668685 ) ) ;
#1330 = VERTEX_POINT ( 'NONE', #12825 ) ;
#1331 = EDGE_LOOP ( 'NONE', ( #7762, #3457, #12304, #16903, #9576 ) ) ;
#1332 = ORIENTED_EDGE ( 'NONE', *, *, #12922, .F. ) ;
#1333 = ADVANCED_FACE ( 'NONE', ( #8924 ), #14465, .F. ) ;
#1334 = CARTESIAN_POINT ( 'NONE',  ( 31.51169109130924184, -2.986371343527201905, 7.939653947423664704 ) ) ;
#1335 = DIRECTION ( 'NONE',  ( 0.000000000000000000, 0.000000000000000000, -1.000000000000000000 ) ) ;
#1336 = VERTEX_POINT ( 'NONE', #17292 ) ;
#1337 = CARTESIAN_POINT ( 'NONE',  ( 31.55553118839817728, -4.235030543236534939, 3.627061608673664228 ) ) ;
#1338 = ORIENTED_EDGE ( 'NONE', *, *, #3322, .F. ) ;
#1339 = DIRECTION ( 'NONE',  ( 1.000000000000000000, 0.000000000000000000, 0.000000000000000000 ) ) ;
#1340 = DIRECTION ( 'NONE',  ( -0.1196152422706611984, 0.9928203230275510771, 0.000000000000000000 ) ) ;
#1341 = CARTESIAN_POINT ( 'NONE',  ( 25.96861057204955259, -6.167300557297518360, -7.540293452860097112 ) ) ;
#1342 = FACE_OUTER_BOUND ( 'NONE', #12131, .T. ) ;
#1343 = CARTESIAN_POINT ( 'NONE',  ( 29.94002636988270538, -4.429666970165102136, -8.283357778048662468 ) ) ;
#1344 = FACE_OUTER_BOUND ( 'NONE', #5620, .T. ) ;
#1345 = EDGE_CURVE ( 'NONE', #15092, #16712, #4429, .T. ) ;
#1346 = DIRECTION ( 'NONE',  ( -0.3420201433256631618, 0.000000000000000000, -0.9396926207859104263 ) ) ;
#1347 = CARTESIAN_POINT ( 'NONE',  ( 28.59583933521957277, -13.42685997174391765, 13.55623838816837079 ) ) ;
#1348 = CARTESIAN_POINT ( 'NONE',  ( 29.78250536075762867, -6.329556739422670830, -6.861505862736167138 ) ) ;
#1349 = CARTESIAN_POINT ( 'NONE',  ( 29.15206445563513071, -6.405512418264540209, -6.861505862736167138 ) ) ;
#1350 = ORIENTED_EDGE ( 'NONE', *, *, #12982, .T. ) ;
#1351 = CARTESIAN_POINT ( 'NONE',  ( 26.01652455409633902, -4.902371455920928156, -5.783357778048663356 ) ) ;
#1352 = CARTESIAN_POINT ( 'NONE',  ( 33.86058074732183343, -3.957317592522819005, 8.111505862736160921 ) ) ;
#1353 = ORIENTED_EDGE ( 'NONE', *, *, #11046, .T. ) ;
#1354 = ORIENTED_EDGE ( 'NONE', *, *, #14243, .T. ) ;
#1355 = ORIENTED_EDGE ( 'NONE', *, *, #14455, .F. ) ;
#1356 = EDGE_CURVE ( 'NONE', #11980, #6730, #14286, .T. ) ;
#1357 = CARTESIAN_POINT ( 'NONE',  ( 31.53813789838894621, -6.745008222462202774, 5.783357778048658915 ) ) ;
#1358 = CARTESIAN_POINT ( 'NONE',  ( 29.01637427789896151, -7.048830937829682064, -5.783357778048668685 ) ) ;
#1359 = LINE ( 'NONE', #11033, #2838 ) ;
#1360 = CARTESIAN_POINT ( 'NONE',  ( 9.750000000000010658, 3.897114317029950037, -3.000000000000002665 ) ) ;
#1361 = CARTESIAN_POINT ( 'NONE',  ( 42.26049544934917179, -5.966988548673008097, -5.783357778048662468 ) ) ;
#1362 = CARTESIAN_POINT ( 'NONE',  ( 30.13703915187255689, -4.405930820630744371, -7.939653947423662039 ) ) ;
#1363 = CARTESIAN_POINT ( 'NONE',  ( 26.10855331130634127, -2.710563430764044490, -4.533357778048659803 ) ) ;
#1364 = DIRECTION ( 'NONE',  ( 0.000000000000000000, 0.000000000000000000, 1.000000000000000000 ) ) ;
#1365 = CARTESIAN_POINT ( 'NONE',  ( 0.000000000000000000, 0.000000000000000000, -10.00000000000000000 ) ) ;
#1366 = EDGE_CURVE ( 'NONE', #10101, #15480, #1791, .T. ) ;
#1367 = CARTESIAN_POINT ( 'NONE',  ( 28.12379965168153362, -6.829206799398704675, -7.033357778048666908 ) ) ;
#1368 = AXIS2_PLACEMENT_3D ( 'NONE', #5699, #11216, #16788 ) ;
#1369 = CARTESIAN_POINT ( 'NONE',  ( -13.00000000000000178, -1.592040838891559293E-15, 10.50000000000000000 ) ) ;
#1370 = CARTESIAN_POINT ( 'NONE',  ( 30.15026255541241440, -6.285249260098253465, -4.705209693361168455 ) ) ;
#1371 = CARTESIAN_POINT ( 'NONE',  ( 36.27615609941022257, -23.17738945083361557, -11.07596365154449636 ) ) ;
#1372 = CARTESIAN_POINT ( 'NONE',  ( 7.958171371211001599, -6.326703190994774850, -2.666481567098319960 ) ) ;
#1373 = CARTESIAN_POINT ( 'NONE',  ( 31.17093069310692499, -6.462087684996337345, 7.033357778048657138 ) ) ;
#1374 = CARTESIAN_POINT ( 'NONE',  ( 0.02511946470933708320, -4.877415451931371493, -3.451298686683631267 ) ) ;
#1375 = AXIS2_PLACEMENT_3D ( 'NONE', #3181, #1841, #8814 ) ;
#1376 = CARTESIAN_POINT ( 'NONE',  ( 27.51889869220010354, -3.467423976192371526, -7.939653947423660263 ) ) ;
#1377 = VERTEX_POINT ( 'NONE', #4564 ) ;
#1378 = EDGE_CURVE ( 'NONE', #7023, #9939, #914, .T. ) ;
#1379 = ORIENTED_EDGE ( 'NONE', *, *, #5330, .F. ) ;
#1380 = ORIENTED_EDGE ( 'NONE', *, *, #3345, .T. ) ;
#1381 = EDGE_CURVE ( 'NONE', #10674, #2813, #10903, .T. ) ;
#1382 = CARTESIAN_POINT ( 'NONE',  ( 4.000000000000000000, 2.309401076758498483, -3.133295621305380863 ) ) ;
#1383 = DIRECTION ( 'NONE',  ( 0.000000000000000000, -1.000000000000000000, -3.469446951953614189E-16 ) ) ;
#1384 = CARTESIAN_POINT ( 'NONE',  ( 9.099998387031005720, -19.29508120620799971, 12.00000000000000000 ) ) ;
#1385 = ORIENTED_EDGE ( 'NONE', *, *, #5413, .F. ) ;
#1386 = AXIS2_PLACEMENT_3D ( 'NONE', #10169, #15444, #5994 ) ;
#1387 = CARTESIAN_POINT ( 'NONE',  ( 31.65190802758064592, -5.477360103042387074, -7.939653947423662927 ) ) ;
#1388 = CARTESIAN_POINT ( 'NONE',  ( 26.64639396487419987, -2.308405637095112706, 5.783357778048667797 ) ) ;
#1389 = UNCERTAINTY_MEASURE_WITH_UNIT (LENGTH_MEASURE( 1.000000000000000082E-05 ), #897, 'distance_accuracy_value', 'NONE');
#1390 = CARTESIAN_POINT ( 'NONE',  ( 26.20620856698912604, -7.060238655668615415, -4.533357778048668685 ) ) ;
#1391 = DIRECTION ( 'NONE',  ( -1.000000000000000000, 0.000000000000000000, 0.000000000000000000 ) ) ;
#1392 = DIRECTION ( 'NONE',  ( 1.000000000000000000, 0.000000000000000000, 0.000000000000000000 ) ) ;
#1393 = AXIS2_PLACEMENT_3D ( 'NONE', #2284, #2110, #15698 ) ;
#1394 = CARTESIAN_POINT ( 'NONE',  ( 27.12922144900085186, -2.887401855662130146, -4.705209693361160461 ) ) ;
#1395 = CARTESIAN_POINT ( 'NONE',  ( 29.14074637024071990, -5.979778010479330774, 8.283357778048660691 ) ) ;
#1396 =( GEOMETRIC_REPRESENTATION_CONTEXT ( 3 ) GLOBAL_UNCERTAINTY_ASSIGNED_CONTEXT ( ( #833 ) ) GLOBAL_UNIT_ASSIGNED_CONTEXT ( ( #16057, #16484, #3972 ) ) REPRESENTATION_CONTEXT ( 'NONE', 'WORKASPACE' ) );
#1397 = CIRCLE ( 'NONE', #8065, 0.8000000000000001554 ) ;
#1398 = EDGE_CURVE ( 'NONE', #9792, #11171, #4666, .T. ) ;
#1399 = CARTESIAN_POINT ( 'NONE',  ( 27.91310269393460430, -7.181753375802955475, 5.783357778048657138 ) ) ;
#1400 = LINE ( 'NONE', #9630, #8117 ) ;
#1401 = CARTESIAN_POINT ( 'NONE',  ( 25.76872643656706074, -21.83605427490913797, 14.29305147543152366 ) ) ;
#1402 = ORIENTED_EDGE ( 'NONE', *, *, #10595, .F. ) ;
#1403 = EDGE_LOOP ( 'NONE', ( #16798, #2310, #7379, #1277 ) ) ;
#1404 = CARTESIAN_POINT ( 'NONE',  ( 27.65467808709180630, -4.705006306174339237, -3.283357778048664688 ) ) ;
#1405 = ORIENTED_EDGE ( 'NONE', *, *, #961, .F. ) ;
#1406 = CARTESIAN_POINT ( 'NONE',  ( 32.90015225647083952, -1.554951264938056132, -5.113484796970854340 ) ) ;
#1407 = CARTESIAN_POINT ( 'NONE',  ( 31.67382807612511542, -6.101689702897060030, -6.861505862736167138 ) ) ;
#1408 = PRODUCT_DEFINITION_CONTEXT ( 'detailed design', #12580, 'design' ) ;
#1409 = DIRECTION ( 'NONE',  ( -0.000000000000000000, -0.000000000000000000, 1.000000000000000000 ) ) ;
#1410 = CARTESIAN_POINT ( 'NONE',  ( -1.917618200156724081E-28, -7.000000000000001776, 6.000000000000000000 ) ) ;
#1411 = CARTESIAN_POINT ( 'NONE',  ( 0.000000000000000000, 0.000000000000000000, 0.000000000000000000 ) ) ;
#1412 = CARTESIAN_POINT ( 'NONE',  ( 34.91600907648203389, -11.88801210197604341, 0.000000000000000000 ) ) ;
#1413 = CARTESIAN_POINT ( 'NONE',  ( 29.01637427789896151, -7.048830937829683840, 5.783357778048658027 ) ) ;
#1414 = CARTESIAN_POINT ( 'NONE',  ( 10.37836969302994028, -0.6704047395399680420, -6.899999999999998579 ) ) ;
#1415 = CARTESIAN_POINT ( 'NONE',  ( 31.63927044622584717, -1.706862622621797110, 6.453230759126472371 ) ) ;
#1416 = CARTESIAN_POINT ( 'NONE',  ( 32.50119254608192421, -4.121097024973739309, 7.939653947423662039 ) ) ;
#1417 = VECTOR ( 'NONE', #15217, 1000.000000000000000 ) ;
#1418 = ORIENTED_EDGE ( 'NONE', *, *, #1366, .T. ) ;
#1419 = AXIS2_PLACEMENT_3D ( 'NONE', #3389, #11806, #15730 ) ;
#1420 = EDGE_CURVE ( 'NONE', #963, #1502, #1958, .T. ) ;
#1421 = VERTEX_POINT ( 'NONE', #13936 ) ;
#1422 = CARTESIAN_POINT ( 'NONE',  ( 29.50659824675005893, -4.481886499472614638, 3.627061608673664228 ) ) ;
#1423 = CARTESIAN_POINT ( 'NONE',  ( -45.50000000000000000, -16.03270077640482683, -2.787981825772262390 ) ) ;
#1424 = ORIENTED_EDGE ( 'NONE', *, *, #11515, .F. ) ;
#1425 = CARTESIAN_POINT ( 'NONE',  ( 27.63266882139180325, -2.199775856772564708, 5.783357778048668685 ) ) ;
#1426 = CARTESIAN_POINT ( 'NONE',  ( 30.71189515440122975, -6.854751018602581958, 5.783357778048664244 ) ) ;
#1427 = CYLINDRICAL_SURFACE ( 'NONE', #8088, 2.499999999999999112 ) ;
#1428 = DIRECTION ( 'NONE',  ( 0.000000000000000000, 0.000000000000000000, -1.000000000000000000 ) ) ;
#1429 = CARTESIAN_POINT ( 'NONE',  ( -4.000000000000000000, 2.309401076758501592, -4.700000000000000178 ) ) ;
#1430 = CARTESIAN_POINT ( 'NONE',  ( 30.05650519998692971, -5.408673599982567026, 13.28483438372752445 ) ) ;
#1431 = AXIS2_PLACEMENT_3D ( 'NONE', #10215, #17040, #3248 ) ;
#1432 = AXIS2_PLACEMENT_3D ( 'NONE', #7668, #3492, #9023 ) ;
#1433 = EDGE_CURVE ( 'NONE', #7967, #2890, #1775, .T. ) ;
#1434 = CARTESIAN_POINT ( 'NONE',  ( 29.49727470010032704, -7.390636972501882340, -5.783357778048669573 ) ) ;
#1435 = CARTESIAN_POINT ( 'NONE',  ( 3.999999999999998224, -2.309401076758513582, -0.5000000000000000000 ) ) ;
#1436 = CARTESIAN_POINT ( 'NONE',  ( 16.96391960790757736, -14.58372395263535282, -16.00480323547922978 ) ) ;
#1437 = CARTESIAN_POINT ( 'NONE',  ( 5.499998817156068753, -20.49639288455253450, 13.00000000000000178 ) ) ;
#1438 = AXIS2_PLACEMENT_3D ( 'NONE', #2614, #17876, #10918 ) ;
#1439 = CARTESIAN_POINT ( 'NONE',  ( 28.39010325924584421, -2.735490497978389612, -4.705209693361160461 ) ) ;
#1440 = CARTESIAN_POINT ( 'NONE',  ( 28.52162355051263987, -6.481468097106410475, -6.861505862736167138 ) ) ;
#1441 = DIRECTION ( 'NONE',  ( 0.000000000000000000, 0.000000000000000000, -1.000000000000000000 ) ) ;
#1442 = FACE_OUTER_BOUND ( 'NONE', #12868, .T. ) ;
#1443 = ORIENTED_EDGE ( 'NONE', *, *, #13426, .T. ) ;
#1444 = CIRCLE ( 'NONE', #7818, 12.50000000000000000 ) ;
#1445 = PRODUCT_DEFINITION_SHAPE ( 'NONE', 'NONE',  #15789 ) ;
#1446 = EDGE_LOOP ( 'NONE', ( #9533, #453, #14937, #5270 ) ) ;
#1447 = CARTESIAN_POINT ( 'NONE',  ( 27.49697864365563760, -2.843094376337701679, 4.705209693361167567 ) ) ;
#1448 = CARTESIAN_POINT ( 'NONE',  ( 28.45891156537951971, -2.090033060632186412, -5.783357778048670461 ) ) ;
#1449 = DIRECTION ( 'NONE',  ( -0.8243186046180107640, 0.5661261679878573094, 0.000000000000000000 ) ) ;
#1450 = VECTOR ( 'NONE', #4216, 1000.000000000000000 ) ;
#1451 = CARTESIAN_POINT ( 'NONE',  ( 25.85239768453567066, -3.540099486550932983, -4.114102314938801186 ) ) ;
#1452 = CARTESIAN_POINT ( 'NONE',  ( 27.71165237056504438, -5.952083095804076684, -7.939653947423664704 ) ) ;
#1453 = FACE_OUTER_BOUND ( 'NONE', #15787, .T. ) ;
#1454 = CARTESIAN_POINT ( 'NONE',  ( 31.89397184978405519, -6.712334120981523711, -5.783357778048663356 ) ) ;
#1455 = CARTESIAN_POINT ( 'NONE',  ( -1.500000000000000000, 10.39230484541326227, -3.000000000000000000 ) ) ;
#1456 = CARTESIAN_POINT ( 'NONE',  ( 30.04891049036066164, -7.324175753722694360, -5.783357778048669573 ) ) ;
#1457 =( BOUNDED_CURVE ( )  B_SPLINE_CURVE ( 2, ( #731, #9330, #13429, #17547, #7893, #9075, #1006, #2458, #11869, #7978, #13514, #814, #17719, #1085, #10509, #14524, #14618, #11777, #7631, #6609, #5240, #15876, #3639, #12139, #7801, #3451, #5067, #7711, #16154, #2107, #6346, #8980, #13152, #16070, #911, #17350, #4887, #10587, #6258, #10417, #3717, #9241, #14787, #2376, #15976, #3544, #17448, #2198, #6531, #11964, #14700, #4982, #13237, #9161, #2282, #12045, #13331, #6445, #17632, #5150, #10669, #16244, #16587, #16338, #12498, #2719, #8240, #13597, #17887, #12589, #3897, #1180, #17807, #5325, #9752, #12235, #10761, #16496, #2885, #13773, #9414, #15039, #9498, #6698, #11481, #13945, #10849, #4169, #7072, #8154, #6968, #16417, #1349, #8412, #13851, #9668, #15216, #5503, #2796, #2533, #168, #11025, #8321, #15305, #1440, #5415, #11108, #13687, #12321, #84, #3982, #2628, #4070, #5591, #16678, #4251, #1539, #14953, #8061, #1273, #6872, #6793, #10930, #9578, #15133, #12403, #14043, #3340, #7160, #12670, #6044, #15576, #15400, #9940, #11287, #1814, #8871, #8591, #16956, #10217, #3073, #1717, #8694, #3155, #4599, #529, #1629, #14222, #262 ),
 .UNSPECIFIED., .F., .T. ) 
 B_SPLINE_CURVE_WITH_KNOTS ( ( 3, 2, 2, 2, 2, 2, 2, 2, 2, 2, 2, 2, 2, 2, 2, 2, 2, 2, 2, 2, 2, 2, 2, 2, 2, 2, 2, 2, 2, 2, 2, 2, 2, 2, 2, 2, 2, 2, 2, 2, 2, 2, 2, 2, 2, 2, 2, 2, 2, 2, 2, 2, 2, 2, 2, 2, 2, 2, 2, 2, 2, 2, 2, 2, 2, 2, 2, 2, 2, 2, 2, 2, 2, 2, 3 ),
 ( 0.000000000000000000, 0.01322951878407230102, 0.02645903756814460203, 0.03968855635221691519, 0.05291807513628920406, 0.06614759392036151375, 0.07937711270443383038, 0.09260663148850611925, 0.1058361502725784081, 0.1190656690566507248, 0.1322951878407230275, 0.1455247066247953303, 0.1587542254088676608, 0.1719837441929399358, 0.1852132629770122385, 0.1984427817610845690, 0.2116723005451568163, 0.2249018193292291468, 0.2381313381133014495, 0.2513608568973737523, 0.2645903756814460550, 0.2778198944655183578, 0.2910494132495906605, 0.3042789320336629633, 0.3175084508177353215, 0.3307379696018076243, 0.3439674883858798715, 0.3571970071699521743, 0.3704265259540244770, 0.3836560447380968353, 0.3968855635221691380, 0.4101150823062413853, 0.4233446010903136325, 0.4365741198743859908, 0.4498036386584582935, 0.4630331574425305963, 0.4762626762266028990, 0.4894921950106752018, 0.5027217137947475045, 0.5159512325788198073, 0.5291807513628921100, 0.5424102701469644128, 0.5556397889310367155, 0.5688693077151090183, 0.5820988264991813210, 0.5953283452832536238, 0.6085578640673259265, 0.6217873828513982293, 0.6350169016354706431, 0.6482464204195428348, 0.6614759392036152486, 0.6747054579876874403, 0.6879349767717597430, 0.7011644955558321568, 0.7143940143399043485, 0.7276235331239767623, 0.7408530519080489540, 0.7540825706921212568, 0.7673120894761936706, 0.7805416082602658623, 0.7937711270443382761, 0.8070006458284105788, 0.8202301646124827705, 0.8334596833965551843, 0.8466892021806272650, 0.8599187209646996788, 0.8731482397487719815, 0.8863777585328441733, 0.8996072773169165870, 0.9128367961009887788, 0.9260663148850611925, 0.9392958336691334953, 0.9525253524532057980, 0.9657548712372781008, 0.9750618896629086318 ),
 .UNSPECIFIED. ) 
 CURVE ( )  GEOMETRIC_REPRESENTATION_ITEM ( )  RATIONAL_B_SPLINE_CURVE ( ( 1.000000000000000000, 0.8660254037844387076, 1.000000000000000000, 0.8660254037844387076, 1.000000000000000000, 0.8660254037844387076, 1.000000000000000000, 0.8660254037844387076, 1.000000000000000000, 0.8660254037844387076, 1.000000000000000000, 0.8660254037844387076, 1.000000000000000000, 0.8660254037844387076, 1.000000000000000000, 0.8660254037844387076, 1.000000000000000000, 0.8660254037844387076, 1.000000000000000000, 0.8660254037844387076, 1.000000000000000000, 0.8660254037844387076, 1.000000000000000000, 0.8660254037844387076, 1.000000000000000000, 0.8660254037844387076, 1.000000000000000000, 0.8660254037844387076, 1.000000000000000000, 0.8660254037844387076, 1.000000000000000000, 0.8660254037844387076, 1.000000000000000000, 0.8660254037844387076, 1.000000000000000000, 0.8660254037844387076, 1.000000000000000000, 0.8660254037844387076, 1.000000000000000000, 0.8660254037844387076, 1.000000000000000000, 0.8660254037844387076, 1.000000000000000000, 0.8660254037844387076, 1.000000000000000000, 0.8660254037844387076, 1.000000000000000000, 0.8660254037844387076, 1.000000000000000000, 0.8660254037844387076, 1.000000000000000000, 0.8660254037844387076, 1.000000000000000000, 0.8660254037844387076, 1.000000000000000000, 0.8660254037844387076, 1.000000000000000000, 0.8660254037844387076, 1.000000000000000000, 0.8660254037844387076, 1.000000000000000000, 0.8660254037844387076, 1.000000000000000000, 0.8660254037844387076, 1.000000000000000000, 0.8660254037844387076, 1.000000000000000000, 0.8660254037844387076, 1.000000000000000000, 0.8660254037844387076, 1.000000000000000000, 0.8660254037844387076, 1.000000000000000000, 0.8660254037844387076, 1.000000000000000000, 0.8660254037844387076, 1.000000000000000000, 0.8660254037844387076, 1.000000000000000000, 0.8660254037844387076, 1.000000000000000000, 0.8660254037844387076, 1.000000000000000000, 0.8660254037844387076, 1.000000000000000000, 0.8660254037844387076, 1.000000000000000000, 0.8660254037844387076, 1.000000000000000000, 0.8660254037844387076, 1.000000000000000000, 0.8660254037844387076, 1.000000000000000000, 0.8660254037844387076, 1.000000000000000000, 0.8660254037844387076, 1.000000000000000000, 0.8660254037844387076, 1.000000000000000000, 0.8660254037844387076, 1.000000000000000000, 0.8660254037844387076, 1.000000000000000000, 0.8660254037844387076, 1.000000000000000000, 0.8660254037844387076, 1.000000000000000000, 0.8660254037844387076, 1.000000000000000000, 0.8660254037844387076, 1.000000000000000000, 0.8660254037844387076, 1.000000000000000000, 0.8660254037844387076, 1.000000000000000000, 0.8660254037844387076, 1.000000000000000000, 0.8660254037844387076, 1.000000000000000000, 0.8660254037844387076, 1.000000000000000000, 0.8660254037844387076, 1.000000000000000000, 0.8660254037844387076, 1.000000000000000000, 0.8660254037844387076, 1.000000000000000000, 0.8660254037844387076, 1.000000000000000000, 0.8660254037844387076, 1.000000000000000000, 0.8660254037844387076, 1.000000000000000000, 0.8660254037844387076, 1.000000000000000000, 0.8660254037844387076, 1.000000000000000000, 0.8660254037844387076, 1.000000000000000000, 0.8660254037844387076, 1.000000000000000000, 0.8660254037844387076, 1.000000000000000000, 0.8660254037844387076, 1.000000000000000000, 0.8660254037844387076, 1.000000000000000000, 0.9057483453558528019, 0.9441095091726994237 ) ) 
 REPRESENTATION_ITEM ( '' )  );
#1458 = ORIENTED_EDGE ( 'NONE', *, *, #501, .T. ) ;
#1459 = EDGE_CURVE ( 'NONE', #8286, #11901, #12912, .T. ) ;
#1460 = CARTESIAN_POINT ( 'NONE',  ( 29.38830135902312080, -2.615227339812091767, -6.861505862736159145 ) ) ;
#1461 = DIRECTION ( 'NONE',  ( -0.000000000000000000, -0.000000000000000000, 1.000000000000000000 ) ) ;
#1462 = PLANE ( 'NONE',  #17617 ) ;
#1463 = DIRECTION ( 'NONE',  ( -0.000000000000000000, -1.000000000000000000, -0.000000000000000000 ) ) ;
#1464 = CARTESIAN_POINT ( 'NONE',  ( 28.51030546511822195, -6.055733689321201041, 8.283357778048660691 ) ) ;
#1465 =( BOUNDED_CURVE ( )  B_SPLINE_CURVE ( 2, ( #17730, #2809, #16350, #3912, #3, #3993, #3826, #14962, #8072 ),
 .UNSPECIFIED., .F., .T. ) 
 B_SPLINE_CURVE_WITH_KNOTS ( ( 3, 2, 2, 2, 3 ),
 ( 0.6346153846153846922, 0.6410256410256410797, 0.6538461538461538547, 0.6666666666666666297, 0.6730769230769231282 ),
 .UNSPECIFIED. ) 
 CURVE ( )  GEOMETRIC_REPRESENTATION_ITEM ( )  RATIONAL_B_SPLINE_CURVE ( ( 0.9330127018922192983, 0.9330127018922198534, 1.000000000000000000, 0.8660254037844387076, 1.000000000000000000, 0.8660254037844387076, 1.000000000000000000, 0.9330127018922187432, 0.9330127018922192983 ) ) 
 REPRESENTATION_ITEM ( '' )  );
#1466 = CARTESIAN_POINT ( 'NONE',  ( 32.47301885516785092, -2.670677813450649474, 8.283357778048664244 ) ) ;
#1467 = CARTESIAN_POINT ( 'NONE',  ( 27.09860475545177039, -3.518061095420291995, -3.627061608673662896 ) ) ;
#1468 = VERTEX_POINT ( 'NONE', #13002 ) ;
#1469 = COLOUR_RGB ( '', 0.72549020, 0.75294118, 0.79215686) ;
#1470 = AXIS2_PLACEMENT_3D ( 'NONE', #15599, #1647, #12691 ) ;
#1471 = DIRECTION ( 'NONE',  ( -0.000000000000000000, -1.000000000000000000, -0.000000000000000000 ) ) ;
#1472 = CARTESIAN_POINT ( 'NONE',  ( -1.499999999999999778, 9.380831519646861238, -2.000000000000000000 ) ) ;
#1473 = VERTEX_POINT ( 'NONE', #14374 ) ;
#1474 = CARTESIAN_POINT ( 'NONE',  ( -21.42089235853292806, -10.15736413759261048, -15.24668633003922658 ) ) ;
#1475 = EDGE_LOOP ( 'NONE', ( #10011, #4500, #155, #17294, #7332 ) ) ;
#1476 = AXIS2_PLACEMENT_3D ( 'NONE', #275, #4265, #2811 ) ;
#1477 = CARTESIAN_POINT ( 'NONE',  ( 29.55043834383900148, -5.730545699181964991, -3.627061608673668225 ) ) ;
#1478 = DIRECTION ( 'NONE',  ( 1.000000000000000000, 0.000000000000000000, 0.000000000000000000 ) ) ;
#1479 = ORIENTED_EDGE ( 'NONE', *, *, #15032, .T. ) ;
#1480 = SHAPE_REPRESENTATION ( 'torque nut 04-2_iso_ISO 7043-M5-N', ( #3575 ), #4782 ) ;
#1481 = EDGE_CURVE ( 'NONE', #9378, #15303, #17106, .T. ) ;
#1482 = CARTESIAN_POINT ( 'NONE',  ( 31.28415083292585663, -5.521667582366822202, -3.627061608673667781 ) ) ;
#1483 = AXIS2_PLACEMENT_3D ( 'NONE', #10857, #17729, #3824 ) ;
#1484 = EDGE_CURVE ( 'NONE', #16203, #1319, #11637, .T. ) ;
#1485 = DIRECTION ( 'NONE',  ( 1.000000000000000000, 0.000000000000000000, 0.000000000000000000 ) ) ;
#1486 = CARTESIAN_POINT ( 'NONE',  ( 4.000000000000000000, -1.677829075513255219, -3.235264651232380828 ) ) ;
#1487 = AXIS2_PLACEMENT_3D ( 'NONE', #6586, #17784, #13491 ) ;
#1488 = CARTESIAN_POINT ( 'NONE',  ( 27.15566825608056689, -6.646038734597135011, -4.705209693361169343 ) ) ;
#1489 = CARTESIAN_POINT ( 'NONE',  ( 21.42986351335030548, -22.27113001973728146, -15.24426822127429659 ) ) ;
#1490 = ORIENTED_EDGE ( 'NONE', *, *, #4667, .T. ) ;
#1491 = CARTESIAN_POINT ( 'NONE',  ( 26.60013260893011378, -1.924431040879551746, 5.783357778048668685 ) ) ;
#1492 = AXIS2_PLACEMENT_3D ( 'NONE', #7438, #13143, #12958 ) ;
#1493 = CARTESIAN_POINT ( 'NONE',  ( 27.04606801335823718, -3.524390735323772006, 3.627061608673666893 ) ) ;
#1494 =( LENGTH_UNIT ( ) NAMED_UNIT ( * ) SI_UNIT ( .MILLI., .METRE. ) );
#1495 = CYLINDRICAL_SURFACE ( 'NONE', #12703, 10.50000000000000000 ) ;
#1496 = AXIS2_PLACEMENT_3D ( 'NONE', #7257, #16878, #15316 ) ;
#1497 = VERTEX_POINT ( 'NONE', #10357 ) ;
#1498 = AXIS2_PLACEMENT_3D ( 'NONE', #7821, #3735, #9092 ) ;
#1499 = CARTESIAN_POINT ( 'NONE',  ( 32.29220775574281532, -1.628196571319322050, -6.453230759126467042 ) ) ;
#1500 = ORIENTED_EDGE ( 'NONE', *, *, #875, .F. ) ;
#1501 = CARTESIAN_POINT ( 'NONE',  ( 27.19802975513453092, -2.241944418315925613, -5.783357778048658027 ) ) ;
#1502 = VERTEX_POINT ( 'NONE', #948 ) ;
#1503 = LINE ( 'NONE', #17936, #9904 ) ;
#1504 = CARTESIAN_POINT ( 'NONE',  ( 27.26074174026764751, -6.633379454790151009, -6.861505862736167138 ) ) ;
#1505 = TOROIDAL_SURFACE ( 'NONE', #14826, 10.40000000000000036, 0.9000000000000003553 ) ;
#1506 = CARTESIAN_POINT ( 'NONE',  ( 31.95146207396702565, -5.641142275435198528, -8.283357778048662468 ) ) ;
#1507 = PLANE ( 'NONE',  #10112 ) ;
#1508 = APPLICATION_PROTOCOL_DEFINITION ( 'draft international standard', 'automotive_design', 1998, #12580 ) ;
#1509 = DIRECTION ( 'NONE',  ( -1.000000000000000000, 0.000000000000000000, 0.000000000000000000 ) ) ;
#1510 = B_SPLINE_CURVE_WITH_KNOTS ( 'NONE', 3,
 ( #5461, #2674, #14995, #1314, #8204, #13731 ),
 .UNSPECIFIED., .F., .F.,
 ( 4, 2, 4 ),
 ( 0.002452478801916373706, 0.003676905084148006115, 0.004901331366379638524 ),
 .UNSPECIFIED. ) ;
#1511 = CARTESIAN_POINT ( 'NONE',  ( 28.99445422935450267, -6.424501337975009996, 4.705209693361160461 ) ) ;
#1512 = EDGE_CURVE ( 'NONE', #11483, #15072, #14540, .T. ) ;
#1513 = CARTESIAN_POINT ( 'NONE',  ( 5.499998817156068753, -20.49639288455253450, 12.00000000000000000 ) ) ;
#1514 = CARTESIAN_POINT ( 'NONE',  ( 27.27683486999669427, -2.232449958253242883, -5.783357778048658027 ) ) ;
#1515 = AXIS2_PLACEMENT_3D ( 'NONE', #6480, #11994, #10616 ) ;
#1516 = CARTESIAN_POINT ( 'NONE',  ( 29.15206445563513071, -6.405512418264540209, 4.705209693361159573 ) ) ;
#1517 = ORIENTED_EDGE ( 'NONE', *, *, #13251, .T. ) ;
#1518 = EDGE_CURVE ( 'NONE', #16729, #10872, #9361, .T. ) ;
#1519 = AXIS2_PLACEMENT_3D ( 'NONE', #14020, #16652, #3133 ) ;
#1520 = CIRCLE ( 'NONE', #12232, 2.749999999999988454 ) ;
#1521 = EDGE_LOOP ( 'NONE', ( #1490, #9810 ) ) ;
#1522 = CARTESIAN_POINT ( 'NONE',  ( 28.87615734162756453, -4.557842178314484016, 3.627061608673664228 ) ) ;
#1523 = CARTESIAN_POINT ( 'NONE',  ( 1.499999999999999778, -9.718191103688257115, -2.333127728361105380 ) ) ;
#1524 = ORIENTED_EDGE ( 'NONE', *, *, #10273, .T. ) ;
#1525 = CARTESIAN_POINT ( 'NONE',  ( 30.45035428628836627, -2.914368949527523789, 3.283357778048666464 ) ) ;
#1526 = ORIENTED_EDGE ( 'NONE', *, *, #7540, .T. ) ;
#1527 = DIRECTION ( 'NONE',  ( 1.000000000000000000, 0.000000000000000000, 0.000000000000000000 ) ) ;
#1528 = DIRECTION ( 'NONE',  ( -0.1196152422706618645, 0.9928203230275510771, 0.000000000000000000 ) ) ;
#1529 = LINE ( 'NONE', #13842, #930 ) ;
#1530 = CARTESIAN_POINT ( 'NONE',  ( 26.65222088368961195, -7.333664733486695120, -5.783357778048669573 ) ) ;
#1531 = CARTESIAN_POINT ( 'NONE',  ( -34.91600907648203389, -11.88801210197604341, -11.56671555609732671 ) ) ;
#1532 = CARTESIAN_POINT ( 'NONE',  ( 28.58911057998038530, -6.046239229258517867, -3.283357778048667797 ) ) ;
#1533 = CARTESIAN_POINT ( 'NONE',  ( 27.11150007966593733, -11.49307575575171469, -13.95470972894434780 ) ) ;
#1534 = CARTESIAN_POINT ( 'NONE',  ( 29.25000000000000000, -16.21813761408365195, 13.37255996287876236 ) ) ;
#1535 = VECTOR ( 'NONE', #2073, 1000.000000000000227 ) ;
#1536 = CARTESIAN_POINT ( 'NONE',  ( 32.02836186724004364, -4.178063784105134459, -7.939653947423662039 ) ) ;
#1537 = ORIENTED_EDGE ( 'NONE', *, *, #3910, .T. ) ;
#1538 = ADVANCED_FACE ( 'NONE', ( #6383 ), #1505, .F. ) ;
#1539 = CARTESIAN_POINT ( 'NONE',  ( 27.89118264539014547, -6.557423775948280742, -6.861505862736167138 ) ) ;
#1540 = CARTESIAN_POINT ( 'NONE',  ( 29.89119874204131122, -2.254829357712824667, -4.533357778048659803 ) ) ;
#1541 = CIRCLE ( 'NONE', #11662, 10.50000000000000000 ) ;
#1542 = ORIENTED_EDGE ( 'NONE', *, *, #7546, .T. ) ;
#1543 = EDGE_CURVE ( 'NONE', #4061, #16703, #10741, .T. ) ;
#1544 = VERTEX_POINT ( 'NONE', #11995 ) ;
#1545 = CARTESIAN_POINT ( 'NONE',  ( 30.27725608814395386, -6.896919580145944195, 5.783357778048658915 ) ) ;
#1546 = CARTESIAN_POINT ( 'NONE',  ( 37.96876116389215383, 4.574485896386907058, 3.995355914169179040E-15 ) ) ;
#1547 = FACE_OUTER_BOUND ( 'NONE', #13456, .T. ) ;
#1548 = CARTESIAN_POINT ( 'NONE',  ( 25.75668387115780078, -2.745663783273349257, -5.690028976746116740 ) ) ;
#1549 = CARTESIAN_POINT ( 'NONE',  ( -5.499998387031001634, -20.49508120620799900, -13.00000000000000178 ) ) ;
#1550 = CARTESIAN_POINT ( 'NONE',  ( 30.65370992780335868, -5.597623261208691581, -3.627061608673667781 ) ) ;
#1551 = CARTESIAN_POINT ( 'NONE',  ( -25.11802603177690330, -16.03270077640482683, 10.53798182577225084 ) ) ;
#1552 = DIRECTION ( 'NONE',  ( 0.000000000000000000, -1.000000000000000000, 0.000000000000000000 ) ) ;
#1553 = DIRECTION ( 'NONE',  ( 0.000000000000000000, 0.000000000000000000, -1.000000000000000000 ) ) ;
#1554 = CARTESIAN_POINT ( 'NONE',  ( 27.38828526237195504, -6.917821758047558056, -4.533357778048668685 ) ) ;
#1555 = ORIENTED_EDGE ( 'NONE', *, *, #12558, .F. ) ;
#1556 = AXIS2_PLACEMENT_3D ( 'NONE', #12533, #15688, #5624 ) ;
#1557 = CARTESIAN_POINT ( 'NONE',  ( 29.64681518302145591, -6.972875258987813574, -5.783357778048668685 ) ) ;
#1558 = CARTESIAN_POINT ( 'NONE',  ( 0.2500000000000002220, 4.898587196589412829E-16, -4.000000000000000000 ) ) ;
#1559 = DIRECTION ( 'NONE',  ( 0.000000000000000000, 3.469446951953614189E-16, -1.000000000000000000 ) ) ;
#1560 = DIRECTION ( 'NONE',  ( 0.9928203230275512992, 0.1196152422706610180, 4.006172263299093133E-17 ) ) ;
#1561 = CARTESIAN_POINT ( 'NONE',  ( 31.03206908560819954, -5.751910973953721751, -3.283357778048667797 ) ) ;
#1562 = CARTESIAN_POINT ( 'NONE',  ( 32.96459815279162342, -1.884545423566157174, 7.033357778048666020 ) ) ;
#1563 = CARTESIAN_POINT ( 'NONE',  ( 29.41022140756759029, -3.239556939666760726, -7.939653947423660263 ) ) ;
#1564 = ORIENTED_EDGE ( 'NONE', *, *, #1138, .T. ) ;
#1565 = ORIENTED_EDGE ( 'NONE', *, *, #5453, .T. ) ;
#1566 = ORIENTED_EDGE ( 'NONE', *, *, #10647, .T. ) ;
#1567 = FACE_OUTER_BOUND ( 'NONE', #7937, .T. ) ;
#1568 = CARTESIAN_POINT ( 'NONE',  ( 0.000000000000000000, 0.000000000000000000, 1.102182119232618281E-16 ) ) ;
#1569 = EDGE_CURVE ( 'NONE', #1274, #12756, #5097, .T. ) ;
#1570 = VERTEX_POINT ( 'NONE', #6290 ) ;
#1571 = CARTESIAN_POINT ( 'NONE',  ( -5.499998387031001634, -20.49508120620799900, -12.00000000000000000 ) ) ;
#1572 = VERTEX_POINT ( 'NONE', #5185 ) ;
#1573 =( BOUNDED_SURFACE ( )  B_SPLINE_SURFACE ( 1, 2, ( 
 ( #12339, #15155, #10777, #3833, #14804, #5258, #13707, #12060, #9430, #14886, #3734, #3917, #2392, #15059, #2472, #13529, #10864, #11981, #10684, #17564, #10605, #16172, #16262, #7908, #13443, #4001, #13616, #9515, #14968, #6813, #1023, #2555, #12256, #5343, #4270, #3174, #12784, #13970, #8, #12518, #15236, #11044, #4530, #8713, #16887, #4185, #188, #16693, #11409, #10048, #2814, #103, #9686, #8528, #16974, #5697, #9771, #8340, #12608, #15509, #6989, #4355, #15324, #16609, #11213, #13873, #9959, #2902, #8433, #5795, #1370, #5611, #5886, #380, #15598, #11126, #1460, #6894, #4449, #3006, #11310, #1557, #3091, #12422, #7090, #5525, #7267, #16787, #9867, #15421, #14060, #1646, #7180, #12689, #282, #8613, #14145, #1735, #17067, #13058, #11596, #6345, #17447, #15694, #12965, #4620, #3450, #4981, #10143, #7629, #10508, #17163, #11868, #8892, #6257, #8979, #17349, #13151, #730, #14523, #11775, #5972, #16069, #4711, #14426, #3543, #3275, #7536, #15784, #3638, #14247, #8808, #2010, #644, #14339, #4886, #10416, #9073, #1925, #15974, #14617, #13236, #7445, #2197, #11496, #2106, #10238, #6167, #11690, #550, #1833, #6067, #3361 ),
 ( #15875, #17260, #7710, #4796, #10318, #813, #7365, #12880, #466, #6608, #13330, #13685, #1178, #9160, #3716, #6444, #13427, #16153, #7977, #17886, #8059, #2532, #1272, #5324, #6792, #6697, #14699, #9240, #11962, #1005, #14786, #13513, #5414, #13596, #12234, #12320, #10848, #2375, #16416, #3981, #17806, #17546, #10929, #6530, #14952, #16495, #5066, #2281, #7799, #10668, #12044, #7892, #1083, #17631, #5149, #910, #9497, #10586, #8153, #12138, #17717, #3814, #16242, #15037, #3896, #9329, #5239, #14868, #2457, #10759, #16337, #9413, #2626, #11453, #11361, #15549, #4168, #16931, #6871, #424, #1348, #4067, #13850, #3130, #5839, #15215, #12734, #9667, #4489, #2718, #2795, #10095, #8239, #8320, #331, #11023, #8664, #14192, #1439, #17020, #10003, #11779, #4574, #13771, #5929, #1785, #12402, #9577, #5501, #6966, #7316, #12836, #16586, #15132, #16238, #1081, #566, #14263, #15713, #13423, #5146, #14865, #3711, #9235, #8731, #10665, #13328, #905, #5988, #10251, #5234, #1853, #11514, #10163, #10583, #1002, #10755, #17628, #6527, #16150, #12135, #5063, #14444, #12041, #8908, #3291, #479, #11615, #17180, #6439, #11960, #7381, #6087 ) ),
 .UNSPECIFIED., .F., .F., .T. ) 
 B_SPLINE_SURFACE_WITH_KNOTS ( ( 2, 2 ),
 ( 3, 2, 2, 2, 2, 2, 2, 2, 2, 2, 2, 2, 2, 2, 2, 2, 2, 2, 2, 2, 2, 2, 2, 2, 2, 2, 2, 2, 2, 2, 2, 2, 2, 2, 2, 2, 2, 2, 2, 2, 2, 2, 2, 2, 2, 2, 2, 2, 2, 2, 2, 2, 2, 2, 2, 2, 2, 2, 2, 2, 2, 2, 2, 2, 2, 2, 2, 2, 2, 2, 2, 2, 2, 2, 2, 2, 3 ),
 ( 0.000000000000000000, 1.000000000000000000 ),
 ( 0.000000000000000000, 0.01282051282051282007, 0.02564102564102564014, 0.03846153846153846367, 0.05128205128205128027, 0.06410256410256409687, 0.07692307692307692735, 0.08974358974358974395, 0.1025641025641025605, 0.1153846153846153910, 0.1282051282051281937, 0.1410256410256410242, 0.1538461538461538547, 0.1666666666666666574, 0.1794871794871794879, 0.1923076923076923184, 0.2051282051282051211, 0.2179487179487179516, 0.2307692307692307820, 0.2435897435897435848, 0.2564102564102563875, 0.2692307692307692180, 0.2820512820512820484, 0.2948717948717948789, 0.3076923076923077094, 0.3205128205128205399, 0.3333333333333333148, 0.3461538461538461453, 0.3589743589743589758, 0.3717948717948718063, 0.3846153846153846367, 0.3974358974358974117, 0.4102564102564102422, 0.4230769230769230727, 0.4358974358974359031, 0.4487179487179487336, 0.4615384615384615641, 0.4743589743589743390, 0.4871794871794871695, 0.5000000000000000000, 0.5128205128205127750, 0.5256410256410256610, 0.5384615384615384359, 0.5512820512820513219, 0.5641025641025640969, 0.5769230769230768718, 0.5897435897435897578, 0.6025641025641025328, 0.6153846153846154188, 0.6282051282051281937, 0.6410256410256410797, 0.6538461538461538547, 0.6666666666666666297, 0.6794871794871795156, 0.6923076923076922906, 0.7051282051282051766, 0.7179487179487179516, 0.7307692307692307265, 0.7435897435897436125, 0.7564102564102563875, 0.7692307692307692735, 0.7820512820512820484, 0.7948717948717948234, 0.8076923076923077094, 0.8205128205128204844, 0.8333333333333333703, 0.8461538461538461453, 0.8589743589743589203, 0.8717948717948718063, 0.8846153846153845812, 0.8974358974358974672, 0.9102564102564102422, 0.9230769230769231282, 0.9358974358974359031, 0.9487179487179486781, 0.9615384615384615641, 0.9690838366659333403 ),
 .UNSPECIFIED. ) 
 GEOMETRIC_REPRESENTATION_ITEM ( )  RATIONAL_B_SPLINE_SURFACE ( (
 ( 1.000000000000000000, 0.8660254037844387076, 1.000000000000000000, 0.8660254037844387076, 1.000000000000000000, 0.8660254037844387076, 1.000000000000000000, 0.8660254037844387076, 1.000000000000000000, 0.8660254037844387076, 1.000000000000000000, 0.8660254037844387076, 1.000000000000000000, 0.8660254037844387076, 1.000000000000000000, 0.8660254037844387076, 1.000000000000000000, 0.8660254037844387076, 1.000000000000000000, 0.8660254037844387076, 1.000000000000000000, 0.8660254037844387076, 1.000000000000000000, 0.8660254037844387076, 1.000000000000000000, 0.8660254037844387076, 1.000000000000000000, 0.8660254037844387076, 1.000000000000000000, 0.8660254037844387076, 1.000000000000000000, 0.8660254037844387076, 1.000000000000000000, 0.8660254037844387076, 1.000000000000000000, 0.8660254037844387076, 1.000000000000000000, 0.8660254037844387076, 1.000000000000000000, 0.8660254037844387076, 1.000000000000000000, 0.8660254037844387076, 1.000000000000000000, 0.8660254037844387076, 1.000000000000000000, 0.8660254037844387076, 1.000000000000000000, 0.8660254037844387076, 1.000000000000000000, 0.8660254037844387076, 1.000000000000000000, 0.8660254037844387076, 1.000000000000000000, 0.8660254037844387076, 1.000000000000000000, 0.8660254037844387076, 1.000000000000000000, 0.8660254037844387076, 1.000000000000000000, 0.8660254037844387076, 1.000000000000000000, 0.8660254037844387076, 1.000000000000000000, 0.8660254037844387076, 1.000000000000000000, 0.8660254037844387076, 1.000000000000000000, 0.8660254037844387076, 1.000000000000000000, 0.8660254037844387076, 1.000000000000000000, 0.8660254037844387076, 1.000000000000000000, 0.8660254037844387076, 1.000000000000000000, 0.8660254037844387076, 1.000000000000000000, 0.8660254037844387076, 1.000000000000000000, 0.8660254037844387076, 1.000000000000000000, 0.8660254037844387076, 1.000000000000000000, 0.8660254037844387076, 1.000000000000000000, 0.8660254037844387076, 1.000000000000000000, 0.8660254037844387076, 1.000000000000000000, 0.8660254037844387076, 1.000000000000000000, 0.8660254037844387076, 1.000000000000000000, 0.8660254037844387076, 1.000000000000000000, 0.8660254037844387076, 1.000000000000000000, 0.8660254037844387076, 1.000000000000000000, 0.8660254037844387076, 1.000000000000000000, 0.8660254037844387076, 1.000000000000000000, 0.8660254037844387076, 1.000000000000000000, 0.8660254037844387076, 1.000000000000000000, 0.8660254037844387076, 1.000000000000000000, 0.8660254037844387076, 1.000000000000000000, 0.8660254037844387076, 1.000000000000000000, 0.8660254037844387076, 1.000000000000000000, 0.8660254037844387076, 1.000000000000000000, 0.8660254037844387076, 1.000000000000000000, 0.8660254037844387076, 1.000000000000000000, 0.8660254037844387076, 1.000000000000000000, 0.8660254037844387076, 1.000000000000000000, 0.8660254037844387076, 1.000000000000000000, 0.8660254037844387076, 1.000000000000000000, 0.8660254037844387076, 1.000000000000000000, 0.8660254037844387076, 1.000000000000000000, 0.8660254037844387076, 1.000000000000000000, 0.8660254037844387076, 1.000000000000000000, 0.8660254037844387076, 1.000000000000000000, 0.8660254037844387076, 1.000000000000000000, 0.8660254037844387076, 1.000000000000000000, 0.8660254037844387076, 1.000000000000000000, 0.8660254037844387076, 1.000000000000000000, 0.8660254037844387076, 1.000000000000000000, 0.8660254037844387076, 1.000000000000000000, 0.9211506902921580142, 0.9351132093492240394),
 ( 1.000000000000000000, 0.8660254037844387076, 1.000000000000000000, 0.8660254037844387076, 1.000000000000000000, 0.8660254037844387076, 1.000000000000000000, 0.8660254037844387076, 1.000000000000000000, 0.8660254037844387076, 1.000000000000000000, 0.8660254037844387076, 1.000000000000000000, 0.8660254037844387076, 1.000000000000000000, 0.8660254037844387076, 1.000000000000000000, 0.8660254037844387076, 1.000000000000000000, 0.8660254037844387076, 1.000000000000000000, 0.8660254037844387076, 1.000000000000000000, 0.8660254037844387076, 1.000000000000000000, 0.8660254037844387076, 1.000000000000000000, 0.8660254037844387076, 1.000000000000000000, 0.8660254037844387076, 1.000000000000000000, 0.8660254037844387076, 1.000000000000000000, 0.8660254037844387076, 1.000000000000000000, 0.8660254037844387076, 1.000000000000000000, 0.8660254037844387076, 1.000000000000000000, 0.8660254037844387076, 1.000000000000000000, 0.8660254037844387076, 1.000000000000000000, 0.8660254037844387076, 1.000000000000000000, 0.8660254037844387076, 1.000000000000000000, 0.8660254037844387076, 1.000000000000000000, 0.8660254037844387076, 1.000000000000000000, 0.8660254037844387076, 1.000000000000000000, 0.8660254037844387076, 1.000000000000000000, 0.8660254037844387076, 1.000000000000000000, 0.8660254037844387076, 1.000000000000000000, 0.8660254037844387076, 1.000000000000000000, 0.8660254037844387076, 1.000000000000000000, 0.8660254037844387076, 1.000000000000000000, 0.8660254037844387076, 1.000000000000000000, 0.8660254037844387076, 1.000000000000000000, 0.8660254037844387076, 1.000000000000000000, 0.8660254037844387076, 1.000000000000000000, 0.8660254037844387076, 1.000000000000000000, 0.8660254037844387076, 1.000000000000000000, 0.8660254037844387076, 1.000000000000000000, 0.8660254037844387076, 1.000000000000000000, 0.8660254037844387076, 1.000000000000000000, 0.8660254037844387076, 1.000000000000000000, 0.8660254037844387076, 1.000000000000000000, 0.8660254037844387076, 1.000000000000000000, 0.8660254037844387076, 1.000000000000000000, 0.8660254037844387076, 1.000000000000000000, 0.8660254037844387076, 1.000000000000000000, 0.8660254037844387076, 1.000000000000000000, 0.8660254037844387076, 1.000000000000000000, 0.8660254037844387076, 1.000000000000000000, 0.8660254037844387076, 1.000000000000000000, 0.8660254037844387076, 1.000000000000000000, 0.8660254037844387076, 1.000000000000000000, 0.8660254037844387076, 1.000000000000000000, 0.8660254037844387076, 1.000000000000000000, 0.8660254037844387076, 1.000000000000000000, 0.8660254037844387076, 1.000000000000000000, 0.8660254037844387076, 1.000000000000000000, 0.8660254037844387076, 1.000000000000000000, 0.8660254037844387076, 1.000000000000000000, 0.8660254037844387076, 1.000000000000000000, 0.8660254037844387076, 1.000000000000000000, 0.8660254037844387076, 1.000000000000000000, 0.8660254037844387076, 1.000000000000000000, 0.8660254037844387076, 1.000000000000000000, 0.8660254037844387076, 1.000000000000000000, 0.8660254037844387076, 1.000000000000000000, 0.8660254037844387076, 1.000000000000000000, 0.8660254037844387076, 1.000000000000000000, 0.8660254037844387076, 1.000000000000000000, 0.8660254037844387076, 1.000000000000000000, 0.8660254037844387076, 1.000000000000000000, 0.8660254037844387076, 1.000000000000000000, 0.8660254037844387076, 1.000000000000000000, 0.8660254037844387076, 1.000000000000000000, 0.9211506902921580142, 0.9351132093492240394) ) ) 
 REPRESENTATION_ITEM ( '' )  SURFACE ( )  );
#1574 = CARTESIAN_POINT ( 'NONE',  ( 30.80679339554874119, -2.444327062417882779, -6.861505862736158257 ) ) ;
#1575 = CARTESIAN_POINT ( 'NONE',  ( 20.00000000000000000, 7.999999999999996447, 15.51150668642334374 ) ) ;
#1576 = ORIENTED_EDGE ( 'NONE', *, *, #5500, .T. ) ;
#1577 = EDGE_LOOP ( 'NONE', ( #14715, #6873, #14999, #11550, #16139 ) ) ;
#1578 = CARTESIAN_POINT ( 'NONE',  ( 30.23341599105502908, -5.648260380436597394, -7.939653947423664704 ) ) ;
#1579 = CYLINDRICAL_SURFACE ( 'NONE', #8368, 2.499999999999999112 ) ;
#1580 = CARTESIAN_POINT ( 'NONE',  ( 5.781152949374531502, 1.605699403978890771, -1.901951201008075243 ) ) ;
#1581 = CARTESIAN_POINT ( 'NONE',  ( 32.22908376348204484, -1.973160382215000785, -7.033357778048658027 ) ) ;
#1582 = ORIENTED_EDGE ( 'NONE', *, *, #8350, .F. ) ;
#1583 = CARTESIAN_POINT ( 'NONE',  ( -20.00000000000000000, 7.999999999999996447, 6.000000000000000000 ) ) ;
#1584 = CARTESIAN_POINT ( 'NONE',  ( 25.61697401368257587, -3.496695820648536568, 8.283357778048664244 ) ) ;
#1585 = EDGE_CURVE ( 'NONE', #2866, #3447, #17811, .T. ) ;
#1586 = CARTESIAN_POINT ( 'NONE',  ( 26.51200394741821498, -4.842675973971495296, 3.627061608673664228 ) ) ;
#1587 = CARTESIAN_POINT ( 'NONE',  ( -27.68843801662522353, -20.37088413741627235, 13.80304640004047023 ) ) ;
#1588 = FACE_OUTER_BOUND ( 'NONE', #14144, .T. ) ;
#1589 = ORIENTED_EDGE ( 'NONE', *, *, #12669, .T. ) ;
#1590 = CARTESIAN_POINT ( 'NONE',  ( 26.30109267735093681, -7.264319738512599933, -6.611283024552371934 ) ) ;
#1591 = ORIENTED_EDGE ( 'NONE', *, *, #13557, .T. ) ;
#1592 = PLANE ( 'NONE',  #14781 ) ;
#1593 =( BOUNDED_CURVE ( )  B_SPLINE_CURVE ( 2, ( #4224, #12834, #15370, #15275, #12644, #7044, #6934, #423, #2953 ),
 .UNSPECIFIED., .F., .T. ) 
 B_SPLINE_CURVE_WITH_KNOTS ( ( 3, 2, 2, 2, 3 ),
 ( 0.01923076923076925265, 0.02564102564102564014, 0.03846153846153846367, 0.05128205128205128027, 0.05769230769230772327 ),
 .UNSPECIFIED. ) 
 CURVE ( )  GEOMETRIC_REPRESENTATION_ITEM ( )  RATIONAL_B_SPLINE_CURVE ( ( 0.9330127018922194093, 0.9330127018922196314, 1.000000000000000000, 0.8660254037844387076, 1.000000000000000000, 0.8660254037844387076, 1.000000000000000000, 0.9330127018922189652, 0.9330127018922192983 ) ) 
 REPRESENTATION_ITEM ( '' )  );
#1594 = ORIENTED_EDGE ( 'NONE', *, *, #2189, .T. ) ;
#1595 = VERTEX_POINT ( 'NONE', #14353 ) ;
#1596 = CARTESIAN_POINT ( 'NONE',  ( 2.749999999999992895, -20.49999999999999645, 6.000000000000000000 ) ) ;
#1597 = CARTESIAN_POINT ( 'NONE',  ( 26.49878054387835746, -2.963357534503999968, -4.705209693361160461 ) ) ;
#1598 = CARTESIAN_POINT ( 'NONE',  ( 32.58190297908952004, -5.565186596593329149, -8.283357778048662468 ) ) ;
#1599 = DIRECTION ( 'NONE',  ( -0.000000000000000000, -1.000000000000000000, -0.000000000000000000 ) ) ;
#1600 = ADVANCED_FACE ( 'NONE', ( #9886 ), #12895, .F. ) ;
#1601 = DIRECTION ( 'NONE',  ( 0.2643151719549537426, 0.9644363586439610447, 0.000000000000000000 ) ) ;
#1602 = FACE_OUTER_BOUND ( 'NONE', #14479, .T. ) ;
#1603 = CARTESIAN_POINT ( 'NONE',  ( 32.08959525433819238, -2.916745304588811649, -7.939653947423660263 ) ) ;
#1604 = DIRECTION ( 'NONE',  ( -0.1196152422706611984, 0.9928203230275511881, 0.000000000000000000 ) ) ;
#1605 = COLOUR_RGB ( '', 0.09019608, 0.27058824, 0.51372549) ;
#1606 = CARTESIAN_POINT ( 'NONE',  ( -45.50000000000000000, -16.03270077640482683, -5.537981825772250843 ) ) ;
#1607 = CARTESIAN_POINT ( 'NONE',  ( 31.06530721954707985, -6.801974981593605030, 5.783357778048657138 ) ) ;
#1608 =( BOUNDED_CURVE ( )  B_SPLINE_CURVE ( 3, ( #6366, #5085, #11796, #10685 ),
 .UNSPECIFIED., .F., .T. ) 
 B_SPLINE_CURVE_WITH_KNOTS ( ( 4, 4 ),
 ( 3.141592653589793116, 6.283185307179586232 ),
 .UNSPECIFIED. ) 
 CURVE ( )  GEOMETRIC_REPRESENTATION_ITEM ( )  RATIONAL_B_SPLINE_CURVE ( ( 1.000000000000000000, 0.3333333333333333703, 0.3333333333333333703, 1.000000000000000000 ) ) 
 REPRESENTATION_ITEM ( '' )  );
#1609 = VERTEX_POINT ( 'NONE', #5715 ) ;
#1610 = EDGE_LOOP ( 'NONE', ( #5758, #2567, #184, #10705, #12070, #3518 ) ) ;
#1611 = EDGE_CURVE ( 'NONE', #11687, #4942, #3105, .T. ) ;
#1612 = CARTESIAN_POINT ( 'NONE',  ( 29.64681518302145591, -6.972875258987813574, 5.783357778048658027 ) ) ;
#1613 = CARTESIAN_POINT ( 'NONE',  ( 31.29094215978502902, -2.813094711071706389, -3.283357778048662023 ) ) ;
#1614 = DIRECTION ( 'NONE',  ( 0.000000000000000000, 1.000000000000000000, -0.000000000000000000 ) ) ;
#1615 = VERTEX_POINT ( 'NONE', #8632 ) ;
#1616 = CARTESIAN_POINT ( 'NONE',  ( 30.41656616297672500, -2.191532958677927745, 4.533357778048667797 ) ) ;
#1617 = ORIENTED_EDGE ( 'NONE', *, *, #4835, .T. ) ;
#1618 = LINE ( 'NONE', #2973, #11821 ) ;
#1619 = CARTESIAN_POINT ( 'NONE',  ( -4.000000000000000888, -1.658477411508030519, -3.231534348142504509 ) ) ;
#1621 = DIRECTION ( 'NONE',  ( 0.9928203230275512992, 0.1196152422706614898, -0.000000000000000000 ) ) ;
#1620 = AXIS2_PLACEMENT_3D ( 'NONE', #12374, #4223, #15191 ) ;
#1622 = DIRECTION ( 'NONE',  ( 1.000000000000000000, 0.000000000000000000, 0.000000000000000000 ) ) ;
#1623 = PLANE ( 'NONE',  #3574 ) ;
#1624 = CARTESIAN_POINT ( 'NONE',  ( 28.55903157092087952, -3.142235986053133256, -8.283357778048658915 ) ) ;
#1625 = CARTESIAN_POINT ( 'NONE',  ( -9.099998387031005720, -19.29508120620799971, -6.000000000000000000 ) ) ;
#1626 = DIRECTION ( 'NONE',  ( 0.000000000000000000, 0.000000000000000000, -1.000000000000000000 ) ) ;
#1627 = CARTESIAN_POINT ( 'NONE',  ( 30.25533603959949502, -6.272589980291270351, -6.861505862736166250 ) ) ;
#1628 = ORIENTED_EDGE ( 'NONE', *, *, #11996, .T. ) ;
#1629 = CARTESIAN_POINT ( 'NONE',  ( 25.86833963875586306, -3.039313213345869791, -4.705209693361160461 ) ) ;
#1630 = LINE ( 'NONE', #7346, #7510 ) ;
#1631 = EDGE_LOOP ( 'NONE', ( #11424, #1747, #3079, #10057 ) ) ;
#1632 = ORIENTED_EDGE ( 'NONE', *, *, #12695, .T. ) ;
#1633 = ORIENTED_EDGE ( 'NONE', *, *, #14529, .F. ) ;
#1634 = ORIENTED_EDGE ( 'NONE', *, *, #10733, .T. ) ;
#1635 = CARTESIAN_POINT ( 'NONE',  ( 28.99445422935450267, -6.424501337975009996, 4.705209693361160461 ) ) ;
#1636 = CARTESIAN_POINT ( 'NONE',  ( 26.21417678486618641, -2.370676134166772808, -5.783357778048658915 ) ) ;
#1637 = CARTESIAN_POINT ( 'NONE',  ( 33.95908713831676096, -3.945449517755638791, -3.283357778048664688 ) ) ;
#1638 = EDGE_CURVE ( 'NONE', #13726, #15016, #7876, .T. ) ;
#1639 = DIRECTION ( 'NONE',  ( 0.7999999999999999334, 0.6000000000000000888, -0.000000000000000000 ) ) ;
#1640 = CARTESIAN_POINT ( 'NONE',  ( 25.71748644841968456, -2.420320648352046078, -5.783357778048663356 ) ) ;
#1641 = CARTESIAN_POINT ( 'NONE',  ( 29.82181869931131146, -4.443908660051686610, -3.627061608673664672 ) ) ;
#1642 = CARTESIAN_POINT ( 'NONE',  ( -2.171643655288370667, 3.365003104552323876, -2.116735335188496547E-15 ) ) ;
#1643 = FACE_OUTER_BOUND ( 'NONE', #7429, .T. ) ;
#1644 = CARTESIAN_POINT ( 'NONE',  ( -2.038300084272748336E-14, -4.618802153517010289, -0.5000000000000000000 ) ) ;
#1645 = CARTESIAN_POINT ( 'NONE',  ( -5.560781378645575757, 6.809993116116508640E-16, -3.700000000000000178 ) ) ;
#1646 = CARTESIAN_POINT ( 'NONE',  ( 28.97253418081003673, -5.800171738120336151, -7.939653947423664704 ) ) ;
#1647 = DIRECTION ( 'NONE',  ( 0.4999999999999921174, -0.8660254037844432595, -0.000000000000000000 ) ) ;
#1648 = FACE_OUTER_BOUND ( 'NONE', #13072, .T. ) ;
#1649 = DIRECTION ( 'NONE',  ( 0.000000000000000000, 1.000000000000000000, 0.000000000000000000 ) ) ;
#1650 = DIRECTION ( 'NONE',  ( 0.7752790601682258975, -0.5233950504778124291, -0.3535533905932748411 ) ) ;
#1651 = CARTESIAN_POINT ( 'NONE',  ( 30.40162818048570514, -5.827866652795590241, 8.283357778048658915 ) ) ;
#1652 = DIRECTION ( 'NONE',  ( 0.9928203230275512992, 0.1196152422706610180, 4.006172263299093133E-17 ) ) ;
#1653 = VERTEX_POINT ( 'NONE', #15613 ) ;
#1654 = CARTESIAN_POINT ( 'NONE',  ( 16.75000000000000000, -16.21813761408365195, -13.00000000000000178 ) ) ;
#1655 = CARTESIAN_POINT ( 'NONE',  ( -1.500000000000000000, 10.05532945112458698, -2.666480854966546854 ) ) ;
#1656 = EDGE_CURVE ( 'NONE', #12969, #2761, #3193, .T. ) ;
#1657 = ORIENTED_EDGE ( 'NONE', *, *, #13824, .T. ) ;
#1658 = DIRECTION ( 'NONE',  ( -1.000000000000000000, 0.000000000000000000, 0.000000000000000000 ) ) ;
#1659 = VERTEX_POINT ( 'NONE', #10600 ) ;
#1660 = CARTESIAN_POINT ( 'NONE',  ( 28.98992747081926069, -3.290194058894681639, -3.627061608673662896 ) ) ;
#1661 = CARTESIAN_POINT ( 'NONE',  ( 26.82722439997946395, -4.804698134550569044, -3.627061608673664672 ) ) ;
#1662 = EDGE_CURVE ( 'NONE', #16642, #4757, #14659, .T. ) ;
#1663 = AXIS2_PLACEMENT_3D ( 'NONE', #7669, #2236, #10710 ) ;
#1664 = CARTESIAN_POINT ( 'NONE',  ( 30.13703915187255689, -4.405930820630744371, -7.939653947423662039 ) ) ;
#1665 = DIRECTION ( 'NONE',  ( 1.000000000000000000, 0.000000000000000000, -0.000000000000000000 ) ) ;
#1666 = DIRECTION ( 'NONE',  ( 0.1196152422706596996, -0.9928203230275514102, 0.000000000000000000 ) ) ;
#1667 = CARTESIAN_POINT ( 'NONE',  ( 31.21213704492286212, -2.822589171134389563, -3.283357778048662023 ) ) ;
#1668 = ADVANCED_FACE ( 'NONE', ( #744 ), #12214, .F. ) ;
#1669 = CARTESIAN_POINT ( 'NONE',  ( 29.91004888286193619, -6.613999042680076990, -4.533357778048668685 ) ) ;
#1670 = VERTEX_POINT ( 'NONE', #7725 ) ;
#1671 = CARTESIAN_POINT ( 'NONE',  ( 32.14213199643172914, -2.910415664685331638, 7.939653947423664704 ) ) ;
#1672 = AXIS2_PLACEMENT_3D ( 'NONE', #7393, #12994, #6000 ) ;
#1673 = EDGE_CURVE ( 'NONE', #11071, #12891, #14799, .T. ) ;
#1674 = CARTESIAN_POINT ( 'NONE',  ( 26.65222088368961195, -7.333664733486695120, 5.783357778048657138 ) ) ;
#1675 = CARTESIAN_POINT ( 'NONE',  ( -29.20851401586840979, -17.04915871481012246, 13.38439546398730329 ) ) ;
#1676 = CARTESIAN_POINT ( 'NONE',  ( 29.77118727536321074, -5.903822331637461396, 8.283357778048660691 ) ) ;
#1677 = EDGE_LOOP ( 'NONE', ( #3552, #11692, #15019, #10159 ) ) ;
#1678 = CARTESIAN_POINT ( 'NONE',  ( 28.55903157092087952, -3.142235986053133256, 3.283357778048666464 ) ) ;
#1679 = ORIENTED_EDGE ( 'NONE', *, *, #11476, .T. ) ;
#1680 = DIRECTION ( 'NONE',  ( 0.000000000000000000, 1.000000000000000000, 0.000000000000000000 ) ) ;
#1681 = EDGE_LOOP ( 'NONE', ( #2872, #12942, #8506, #11459 ) ) ;
#1682 = CARTESIAN_POINT ( 'NONE',  ( 26.67454832010805532, -2.305013593294074514, -5.113484796970851676 ) ) ;
#1683 = CARTESIAN_POINT ( 'NONE',  ( 33.83155592109562804, -6.868441680671474536, -5.783357778048669573 ) ) ;
#1684 = CARTESIAN_POINT ( 'NONE',  ( 32.61569110240115776, -6.288022587442930522, -7.033357778048666908 ) ) ;
#1685 = CARTESIAN_POINT ( 'NONE',  ( 33.50243880635947846, -1.482387629897225390, 5.783357778048663356 ) ) ;
#1686 = CARTESIAN_POINT ( 'NONE',  ( -22.99999999999999645, -16.21813761408365195, 17.69999999999999574 ) ) ;
#1687 = DIRECTION ( 'NONE',  ( 0.000000000000000000, 0.000000000000000000, 1.000000000000000000 ) ) ;
#1688 = CARTESIAN_POINT ( 'NONE',  ( 32.81641299864316608, -4.083119185552795294, -7.939653947423662039 ) ) ;
#1689 = EDGE_CURVE ( 'NONE', #4375, #14985, #834, .T. ) ;
#1690 = CYLINDRICAL_SURFACE ( 'NONE', #4990, 2.500000000000001776 ) ;
#1692 = VECTOR ( 'NONE', #7368, 1000.000000000000000 ) ;
#1691 = CARTESIAN_POINT ( 'NONE',  ( 32.29295089585318834, -5.599999616269981217, 8.283357778048660691 ) ) ;
#1693 = CARTESIAN_POINT ( 'NONE',  ( 31.24031073583692475, -4.273008382657478954, 7.939653947423662039 ) ) ;
#1694 = ORIENTED_EDGE ( 'NONE', *, *, #10152, .T. ) ;
#1695 =( BOUNDED_CURVE ( )  B_SPLINE_CURVE ( 2, ( #5317, #3629, #900, #16145, #10750, #2522, #17878, #6688, #12221 ),
 .UNSPECIFIED., .F., .T. ) 
 B_SPLINE_CURVE_WITH_KNOTS ( ( 3, 2, 2, 2, 3 ),
 ( 0.7115384615384615641, 0.7179487179487179516, 0.7307692307692307265, 0.7435897435897436125, 0.7500000000000000000 ),
 .UNSPECIFIED. ) 
 CURVE ( )  GEOMETRIC_REPRESENTATION_ITEM ( )  RATIONAL_B_SPLINE_CURVE ( ( 0.9330127018922194093, 0.9330127018922194093, 1.000000000000000000, 0.8660254037844387076, 1.000000000000000000, 0.8660254037844387076, 1.000000000000000000, 0.9330127018922194093, 0.9330127018922194093 ) ) 
 REPRESENTATION_ITEM ( '' )  );
#1696 = ORIENTED_EDGE ( 'NONE', *, *, #592, .T. ) ;
#1697 = CARTESIAN_POINT ( 'NONE',  ( 27.49697864365563760, -2.843094376337701679, 4.705209693361167567 ) ) ;
#1698 = DIRECTION ( 'NONE',  ( -1.000000000000000000, 0.000000000000000000, 0.000000000000000000 ) ) ;
#1699 = CARTESIAN_POINT ( 'NONE',  ( 1.499999999999999778, -9.380831519646861238, -2.000000000000000000 ) ) ;
#1700 = EDGE_CURVE ( 'NONE', #17480, #7830, #17463, .T. ) ;
#1701 = VERTEX_POINT ( 'NONE', #13439 ) ;
#1702 = CARTESIAN_POINT ( 'NONE',  ( 30.71189515440122975, -6.854751018602581958, 5.783357778048664244 ) ) ;
#1703 = ORIENTED_EDGE ( 'NONE', *, *, #9712, .F. ) ;
#1704 = DIRECTION ( 'NONE',  ( 0.9899494936611662466, 0.1414213562373111965, 0.000000000000000000 ) ) ;
#1705 = CARTESIAN_POINT ( 'NONE',  ( -50.00000000000000000, -19.03270077640483038, -5.537981825772250843 ) ) ;
#1706 = FACE_OUTER_BOUND ( 'NONE', #10911, .T. ) ;
#1707 = CARTESIAN_POINT ( 'NONE',  ( 0.2500000000000002220, 0.000000000000000000, 0.000000000000000000 ) ) ;
#1708 =( REPRESENTATION_RELATIONSHIP ('NONE','NONE', #3227, #12598 ) REPRESENTATION_RELATIONSHIP_WITH_TRANSFORMATION ( #15824 )SHAPE_REPRESENTATION_RELATIONSHIP( ) );
#1709 = CARTESIAN_POINT ( 'NONE',  ( 25.90934487712387480, 0.1208734971681818676, -4.216642221951339309 ) ) ;
#1710 = CARTESIAN_POINT ( 'NONE',  ( 27.29814976067589072, -3.294147343736873346, -8.283357778048658915 ) ) ;
#1711 = CARTESIAN_POINT ( 'NONE',  ( 32.97895737133300287, -1.545456804875373402, -5.113484796970854340 ) ) ;
#1712 = CYLINDRICAL_SURFACE ( 'NONE', #15739, 5.000000000000000000 ) ;
#1713 = CARTESIAN_POINT ( 'NONE',  ( 30.76748005699505129, -4.329975141788874993, -7.939653947423662039 ) ) ;
#1714 = CONICAL_SURFACE ( 'NONE', #17075, 3.999999999999986677, 0.7853981633974400633 ) ;
#1715 = ADVANCED_FACE ( 'NONE', ( #10335 ), #17464, .F. ) ;
#1716 = EDGE_CURVE ( 'NONE', #17066, #14839, #5080, .T. ) ;
#1717 = CARTESIAN_POINT ( 'NONE',  ( 26.65222088368961195, -7.333664733486695120, -5.783357778048669573 ) ) ;
#1718 = CARTESIAN_POINT ( 'NONE',  ( 27.02423718196931546, -4.780961985016209503, -3.283357778048664688 ) ) ;
#1719 = ORIENTED_EDGE ( 'NONE', *, *, #14326, .F. ) ;
#1720 = ORIENTED_EDGE ( 'NONE', *, *, #10977, .T. ) ;
#1721 = ORIENTED_EDGE ( 'NONE', *, *, #9838, .F. ) ;
#1722 = CARTESIAN_POINT ( 'NONE',  ( 28.73594040535617467, -2.066853418799292630, 5.783357778048668685 ) ) ;
#1723 = CONICAL_SURFACE ( 'NONE', #8085, 5.560781378645573980, 1.221730476396047926 ) ;
#1724 = LINE ( 'NONE', #7254, #3871 ) ;
#1725 = DIRECTION ( 'NONE',  ( -0.9928203230275511881, -0.1196152422706606572, -1.761484381769779444E-15 ) ) ;
#1726 = DIRECTION ( 'NONE',  ( -0.9928203230275510771, -0.1196152422706610735, 0.000000000000000000 ) ) ;
#1727 = FACE_OUTER_BOUND ( 'NONE', #3816, .T. ) ;
#1728 = CARTESIAN_POINT ( 'NONE',  ( 25.72395281601508898, -4.937620572523835349, -7.939653947423662039 ) ) ;
#1729 = CARTESIAN_POINT ( 'NONE',  ( 31.29094215978502902, -2.813094711071706389, -3.283357778048662023 ) ) ;
#1730 = DIRECTION ( 'NONE',  ( 0.000000000000000000, 0.000000000000000000, -1.000000000000000000 ) ) ;
#1731 = CIRCLE ( 'NONE', #11847, 2.000000000000001776 ) ;
#1732 = CARTESIAN_POINT ( 'NONE',  ( 13.00000000000000178, 0.000000000000000000, 6.000000000000000000 ) ) ;
#1733 = UNCERTAINTY_MEASURE_WITH_UNIT (LENGTH_MEASURE( 1.000000000000000082E-05 ), #3980, 'distance_accuracy_value', 'NONE');
#1734 = CARTESIAN_POINT ( 'NONE',  ( 27.80031630502317341, -2.169380783275094426, -6.453230759126464378 ) ) ;
#1735 = CARTESIAN_POINT ( 'NONE',  ( 28.35948656569675919, -3.366149737736551906, -3.627061608673662896 ) ) ;
#1736 = CARTESIAN_POINT ( 'NONE',  ( 26.01652455409633902, -4.902371455920926380, 5.783357778048663356 ) ) ;
#1737 = CARTESIAN_POINT ( 'NONE',  ( 32.34851646621051202, -1.621412483717243447, -5.113484796970854340 ) ) ;
#1738 = CARTESIAN_POINT ( 'NONE',  ( -8.776279441628744848, 6.799038105676760146, -11.72793873352925331 ) ) ;
#1739 = B_SPLINE_CURVE_WITH_KNOTS ( 'NONE', 3,
 ( #15486, #8503, #8586, #15572, #17039, #1983, #10116, #15666, #3336, #11568, #8866, #14399, #7506, #15393, #2981, #1401, #9374, #6753, #1132, #1052, #13642, #5289, #8018, #14915, #2583, #2495, #16294, #9294, #17932, #41, #2765, #1232, #12284, #16381, #6573, #10982, #16460, #6921, #8110, #11075, #14834, #9631, #6658 ),
 .UNSPECIFIED., .F., .F.,
 ( 4, 2, 2, 1, 2, 2, 2, 2, 2, 2, 2, 2, 2, 2, 2, 2, 2, 2, 2, 2, 2, 4 ),
 ( 0.01976987703536532692, 0.02100501831352976842, 0.02162258895261198396, 0.02224015959169420298, 0.02285773023077641852, 0.02347530086985863407, 0.02471044214802306516, 0.02594558342618749971, 0.02718072470435193080, 0.02779829534343414288, 0.02841586598251635495, 0.02965100726068079298, 0.03088614853884522754, 0.03150371917792745002, 0.03212128981700967945, 0.03335643109517413829, 0.03459157237333859714, 0.03582671365150305598, 0.03644428429058528540, 0.03706185492966751482, 0.03829699620783197367, 0.03953213748599642557 ),
 .UNSPECIFIED. ) ;
#1740 = AXIS2_PLACEMENT_3D ( 'NONE', #5863, #7155, #11283 ) ;
#1741 = CIRCLE ( 'NONE', #10673, 14.00000000000000178 ) ;
#1742 = CARTESIAN_POINT ( 'NONE',  ( 26.82229025357024454, -7.323371595517525812, 6.453230759126462601 ) ) ;
#1743 = ADVANCED_FACE ( 'NONE', ( #15891 ), #14883, .T. ) ;
#1744 = CARTESIAN_POINT ( 'NONE',  ( 27.81599742762458050, -2.504850134108091098, 4.533357778048667797 ) ) ;
#1745 = CARTESIAN_POINT ( 'NONE',  ( 1.500000000000000666, 5.809475019311125976, -3.000000000000000000 ) ) ;
#1746 = AXIS2_PLACEMENT_3D ( 'NONE', #7236, #16945, #11562 ) ;
#1747 = ORIENTED_EDGE ( 'NONE', *, *, #9946, .T. ) ;
#1748 = ADVANCED_FACE ( 'NONE', ( #3831 ), #7240, .F. ) ;
#1749 = CYLINDRICAL_SURFACE ( 'NONE', #2139, 2.500000000000001776 ) ;
#1750 = CARTESIAN_POINT ( 'NONE',  ( 45.50000000000000000, -19.03270077640483038, -5.537981825772250843 ) ) ;
#1751 = ORIENTED_EDGE ( 'NONE', *, *, #14289, .F. ) ;
#1752 = CARTESIAN_POINT ( 'NONE',  ( -19.91444112663254984, -10.77903654349075246, -15.52697452096630748 ) ) ;
#1753 = ORIENTED_EDGE ( 'NONE', *, *, #14588, .F. ) ;
#1754 = AXIS2_PLACEMENT_3D ( 'NONE', #2951, #1599, #1782 ) ;
#1755 = CARTESIAN_POINT ( 'NONE',  ( 27.02414796481377124, -2.900061135469103490, -6.861505862736158257 ) ) ;
#1756 = CARTESIAN_POINT ( 'NONE',  ( 31.93198502805756789, -2.935734224299280548, -7.939653947423660263 ) ) ;
#1757 = PLANE ( 'NONE',  #3505 ) ;
#1758 = DIRECTION ( 'NONE',  ( 0.000000000000000000, 0.000000000000000000, 1.000000000000000000 ) ) ;
#1759 = DIRECTION ( 'NONE',  ( -1.000000000000000000, 0.000000000000000000, -0.000000000000000000 ) ) ;
#1760 = CARTESIAN_POINT ( 'NONE',  ( 31.27600417729400917, -6.449428405189353342, -7.033357778048666908 ) ) ;
#1761 = EDGE_CURVE ( 'NONE', #6497, #8021, #12796, .T. ) ;
#1762 = CARTESIAN_POINT ( 'NONE',  ( 29.35089333861488115, -5.954459450865362768, -8.283357778048664244 ) ) ;
#1763 = VECTOR ( 'NONE', #10981, 1000.000000000000114 ) ;
#1764 = EDGE_LOOP ( 'NONE', ( #11987, #7396, #5644, #9866, #15153 ) ) ;
#1765 = CARTESIAN_POINT ( 'NONE',  ( 32.64557936882268052, -2.222789665795767089, 6.861505862736165362 ) ) ;
#1766 = CIRCLE ( 'NONE', #17732, 2.500000000000000888 ) ;
#1767 = EDGE_CURVE ( 'NONE', #2633, #13499, #4683, .T. ) ;
#1768 = CARTESIAN_POINT ( 'NONE',  ( 0.000000000000000000, 0.000000000000000000, -2.000000000000000000 ) ) ;
#1769 = CARTESIAN_POINT ( 'NONE',  ( -16.96458082634299558, -17.85487492059188597, 16.00470661676384054 ) ) ;
#1770 = CARTESIAN_POINT ( 'NONE',  ( 2.749999999999992895, -20.49999999999999645, -6.000000000000000000 ) ) ;
#1771 = ORIENTED_EDGE ( 'NONE', *, *, #6840, .T. ) ;
#1772 = DIRECTION ( 'NONE',  ( 1.224646799147353207E-16, -1.000000000000000000, 0.000000000000000000 ) ) ;
#1773 = EDGE_LOOP ( 'NONE', ( #5510, #13248, #5935, #4030 ) ) ;
#1774 = DIRECTION ( 'NONE',  ( -0.1196152422706609625, 0.9928203230275510771, -4.694733121053619507E-17 ) ) ;
#1775 = LINE ( 'NONE', #11444, #15386 ) ;
#1776 = ORIENTED_EDGE ( 'NONE', *, *, #17144, .T. ) ;
#1777 = CARTESIAN_POINT ( 'NONE',  ( 26.90793483298705979, -6.248787706170159773, -8.283357778048664244 ) ) ;
#1778 = VECTOR ( 'NONE', #16902, 1000.000000000000000 ) ;
#1779 = AXIS2_PLACEMENT_3D ( 'NONE', #16654, #16311, #6853 ) ;
#1780 = CARTESIAN_POINT ( 'NONE',  ( 26.60838078660069428, -6.085005533777348319, -7.939653947423664704 ) ) ;
#1781 = CARTESIAN_POINT ( 'NONE',  ( 31.83134908525019213, -4.201799933639492224, -8.283357778048662468 ) ) ;
#1782 = DIRECTION ( 'NONE',  ( 0.000000000000000000, 0.000000000000000000, -1.000000000000000000 ) ) ;
#1783 = PRODUCT_CONTEXT ( 'NONE', #5262, 'mechanical' ) ;
#1784 = DIRECTION ( 'NONE',  ( -1.000000000000000000, 0.000000000000000000, 0.000000000000000000 ) ) ;
#1785 = CARTESIAN_POINT ( 'NONE',  ( 28.54354359905709870, -7.105797696961086096, -5.783357778048669573 ) ) ;
#1786 = DIRECTION ( 'NONE',  ( -0.8660254037844397068, -0.4999999999999981126, 0.000000000000000000 ) ) ;
#1787 = VECTOR ( 'NONE', #1827, 1000.000000000000000 ) ;
#1788 = DIRECTION ( 'NONE',  ( -0.1196152422706610735, 0.9928203230275511881, 0.000000000000000000 ) ) ;
#1789 = CARTESIAN_POINT ( 'NONE',  ( 20.00000000000000355, 7.999999999999996447, 0.000000000000000000 ) ) ;
#1790 = CARTESIAN_POINT ( 'NONE',  ( 29.13014440709066832, -5.781182818409868140, 3.627061608673662896 ) ) ;
#1791 =( BOUNDED_CURVE ( )  B_SPLINE_CURVE ( 3, ( #6007, #677, #1872, #6201 ),
 .UNSPECIFIED., .F., .T. ) 
 B_SPLINE_CURVE_WITH_KNOTS ( ( 4, 4 ),
 ( 4.889642689481717319, 5.052230418047667371 ),
 .UNSPECIFIED. ) 
 CURVE ( )  GEOMETRIC_REPRESENTATION_ITEM ( )  RATIONAL_B_SPLINE_CURVE ( ( 1.000000000000000000, 0.9977983154653931042, 0.9977983154653931042, 1.000000000000000000 ) ) 
 REPRESENTATION_ITEM ( '' )  );
#1792 = ORIENTED_EDGE ( 'NONE', *, *, #15004, .T. ) ;
#1793 = CONICAL_SURFACE ( 'NONE', #9020, 3.999999999999986677, 0.7853981633974400633 ) ;
#1794 = CARTESIAN_POINT ( 'NONE',  ( 26.88845778707760914, -3.543379655034240905, -7.939653947423660263 ) ) ;
#1795 = ORIENTED_EDGE ( 'NONE', *, *, #16836, .F. ) ;
#1796 = CARTESIAN_POINT ( 'NONE',  ( 28.25893984004492765, -6.513116296623863377, 6.861505862736158257 ) ) ;
#1797 = CARTESIAN_POINT ( 'NONE',  ( 31.15208055228630357, -2.102918000029084578, -4.533357778048659803 ) ) ;
#1798 = CARTESIAN_POINT ( 'NONE',  ( -10.37836969302994028, 0.6704047395399693743, -6.899999999999998579 ) ) ;
#1799 = ORIENTED_EDGE ( 'NONE', *, *, #8255, .T. ) ;
#1800 = CARTESIAN_POINT ( 'NONE',  ( 25.86833963875586306, -3.039313213345869791, 6.861505862736166250 ) ) ;
#1801 = ORIENTED_EDGE ( 'NONE', *, *, #8627, .T. ) ;
#1802 = AXIS2_PLACEMENT_3D ( 'NONE', #10064, #17179, #202 ) ;
#1803 = CARTESIAN_POINT ( 'NONE',  ( 47.10521669518294630, -4.378041487036768764, -5.783357778048661579 ) ) ;
#1804 = EDGE_CURVE ( 'NONE', #5110, #16117, #13702, .T. ) ;
#1805 = CARTESIAN_POINT ( 'NONE',  ( -1.917618200156724081E-28, -7.000000000000001776, 0.000000000000000000 ) ) ;
#1806 = CARTESIAN_POINT ( 'NONE',  ( 2.500000000000000000, 0.000000000000000000, 0.000000000000000000 ) ) ;
#1807 = CARTESIAN_POINT ( 'NONE',  ( 4.000000000000000000, -2.309401076758510918, -3.133295621305383083 ) ) ;
#1808 = CARTESIAN_POINT ( 'NONE',  ( 33.14902674121363901, -1.535163666906202318, -5.783357778048658027 ) ) ;
#1809 = PLANE ( 'NONE',  #1136 ) ;
#1810 = AXIS2_PLACEMENT_3D ( 'NONE', #6953, #1621, #1340 ) ;
#1811 = CARTESIAN_POINT ( 'NONE',  ( 2.500000000000000000, 2.500728763858895382E-16, -2.041999999999999815 ) ) ;
#1812 =( LENGTH_UNIT ( ) NAMED_UNIT ( * ) SI_UNIT ( .MILLI., .METRE. ) );
#1813 = CARTESIAN_POINT ( 'NONE',  ( 30.25080928106424594, -3.138282701210941994, -3.627061608673662896 ) ) ;
#1814 = CARTESIAN_POINT ( 'NONE',  ( 26.37178701114681800, -2.351687214456304797, -5.783357778048658915 ) ) ;
#1815 = CARTESIAN_POINT ( 'NONE',  ( 29.79859849048667897, -1.928627242885762705, -5.783357778048664244 ) ) ;
#1816 = VECTOR ( 'NONE', #17366, 1000.000000000000000 ) ;
#1817 = ORIENTED_EDGE ( 'NONE', *, *, #14108, .F. ) ;
#1818 = EDGE_LOOP ( 'NONE', ( #15282, #13982, #15252, #337 ) ) ;
#1819 = VERTEX_POINT ( 'NONE', #9425 ) ;
#1820 = CARTESIAN_POINT ( 'NONE',  ( 27.47505859511117521, -2.218764776483033163, 5.783357778048668685 ) ) ;
#1821 = CARTESIAN_POINT ( 'NONE',  ( 39.99999999999999289, 0.000000000000000000, 2.055000000000000160 ) ) ;
#1822 = FACE_OUTER_BOUND ( 'NONE', #10493, .T. ) ;
#1823 = CARTESIAN_POINT ( 'NONE',  ( -19.49912934580633106, 8.667827538924893105, -15.60122950519025409 ) ) ;
#1824 = EDGE_CURVE ( 'NONE', #17674, #12357, #5, .T. ) ;
#1825 = CARTESIAN_POINT ( 'NONE',  ( -28.59532824046058153, -19.01044845393195715, -13.55637998813296186 ) ) ;
#1826 = CARTESIAN_POINT ( 'NONE',  ( 26.03917326857634151, -4.899642733102906433, -3.627061608673664672 ) ) ;
#1827 = DIRECTION ( 'NONE',  ( -0.000000000000000000, -0.000000000000000000, -1.000000000000000000 ) ) ;
#1828 = CARTESIAN_POINT ( 'NONE',  ( 26.01652455409633902, -4.902371455920926380, -5.783357778048663356 ) ) ;
#1829 = CIRCLE ( 'NONE', #10767, 2.000000000000001776 ) ;
#1830 = LINE ( 'NONE', #17063, #3240 ) ;
#1831 = CARTESIAN_POINT ( 'NONE',  ( 26.14503574297738098, -5.691300421908874085, -8.283357778048664244 ) ) ;
#1832 = ORIENTED_EDGE ( 'NONE', *, *, #5500, .F. ) ;
#1833 = CARTESIAN_POINT ( 'NONE',  ( 25.72395281601508898, -4.937620572523835349, -7.939653947423662039 ) ) ;
#1834 = CONICAL_SURFACE ( 'NONE', #7613, 3.425051884552432480, 0.7853981633974544962 ) ;
#1835 = DIRECTION ( 'NONE',  ( 0.000000000000000000, 1.000000000000000000, 3.469446951953614189E-16 ) ) ;
#1836 = CARTESIAN_POINT ( 'NONE',  ( 35.19141017012124451, -14.17387298022714326, 11.46934516270796323 ) ) ;
#1837 = LINE ( 'NONE', #9962, #1692 ) ;
#1838 = DIRECTION ( 'NONE',  ( 0.05980762113533042573, -0.4964101615137759826, 0.8660254037844383745 ) ) ;
#1839 = VECTOR ( 'NONE', #13387, 999.9999999999998863 ) ;
#1840 = CARTESIAN_POINT ( 'NONE',  ( 30.01512236704901682, -6.601339762873093875, 4.533357778048659803 ) ) ;
#1841 = DIRECTION ( 'NONE',  ( 0.000000000000000000, -0.000000000000000000, 1.000000000000000000 ) ) ;
#1842 = VECTOR ( 'NONE', #5538, 1000.000000000000000 ) ;
#1843 = AXIS2_PLACEMENT_3D ( 'NONE', #12222, #9657, #2789 ) ;
#1844 = ORIENTED_EDGE ( 'NONE', *, *, #1716, .F. ) ;
#1845 = VERTEX_POINT ( 'NONE', #6808 ) ;
#1846 = EDGE_CURVE ( 'NONE', #16993, #17950, #4103, .T. ) ;
#1847 = VERTEX_POINT ( 'NONE', #13871 ) ;
#1848 = CARTESIAN_POINT ( 'NONE',  ( -17.40654580017221065, -13.42197210625884551, -15.93919332483364748 ) ) ;
#1849 = CIRCLE ( 'NONE', #1431, 10.50000000000000000 ) ;
#1850 = EDGE_CURVE ( 'NONE', #16681, #13069, #16352, .T. ) ;
#1851 = EDGE_LOOP ( 'NONE', ( #4202, #12524, #6400, #11426 ) ) ;
#1852 = CARTESIAN_POINT ( 'NONE',  ( 27.89118264539014547, -6.557423775948280742, -6.861505862736167138 ) ) ;
#1853 = CARTESIAN_POINT ( 'NONE',  ( 27.02867472334902033, -6.034368414549446058, -3.627061608673668225 ) ) ;
#1854 = CARTESIAN_POINT ( 'NONE',  ( 29.60297508593253468, -5.724216059278466773, -7.939653947423664704 ) ) ;
#1855 = ORIENTED_EDGE ( 'NONE', *, *, #17095, .F. ) ;
#1856 = CARTESIAN_POINT ( 'NONE',  ( 27.80031630502317341, -2.169380783275094426, -6.453230759126464378 ) ) ;
#1857 = CARTESIAN_POINT ( 'NONE',  ( 28.48706592061337162, -2.086641016831144668, -5.113484796970857893 ) ) ;
#1858 = CARTESIAN_POINT ( 'NONE',  ( -1.917618200156724081E-28, -7.000000000000001776, 6.000000000000000000 ) ) ;
#1859 = CARTESIAN_POINT ( 'NONE',  ( 31.03206908560819954, -5.751910973953720863, -3.283357778048667797 ) ) ;
#1860 = CARTESIAN_POINT ( 'NONE',  ( 29.37220822929407760, -7.016156836349003001, -5.783357778048668685 ) ) ;
#1861 = CARTESIAN_POINT ( 'NONE',  ( 33.42946061375642586, -6.517141185936593750, 5.783357778048658027 ) ) ;
#1862 = CIRCLE ( 'NONE', #6762, 9.500000000000000000 ) ;
#1863 = AXIS2_PLACEMENT_3D ( 'NONE', #15659, #6311, #2165 ) ;
#1864 = CARTESIAN_POINT ( 'NONE',  ( 31.24973580796908834, -6.452593224933654170, 7.033357778048657138 ) ) ;
#1865 = CARTESIAN_POINT ( 'NONE',  ( -17.59998316743469715, -19.37170218437266200, 15.90983619775817459 ) ) ;
#1866 = LINE ( 'NONE', #11348, #561 ) ;
#1867 = ORIENTED_EDGE ( 'NONE', *, *, #13233, .T. ) ;
#1868 = FACE_OUTER_BOUND ( 'NONE', #16030, .T. ) ;
#1869 = VERTEX_POINT ( 'NONE', #1455 ) ;
#1870 = DIRECTION ( 'NONE',  ( 1.000000000000000000, 0.000000000000000000, -0.000000000000000000 ) ) ;
#1871 = EDGE_CURVE ( 'NONE', #9271, #10223, #12515, .T. ) ;
#1872 = CARTESIAN_POINT ( 'NONE',  ( -30.05650519998691195, -5.408673599982547486, 13.28483438372753156 ) ) ;
#1873 = ORIENTED_EDGE ( 'NONE', *, *, #9077, .F. ) ;
#1874 = LINE ( 'NONE', #7403, #10487 ) ;
#1875 = CIRCLE ( 'NONE', #3312, 2.500000000000000000 ) ;
#1876 = CARTESIAN_POINT ( 'NONE',  ( 31.64365984991007252, -1.316785610144591390, -5.783357778048658027 ) ) ;
#1877 = CARTESIAN_POINT ( 'NONE',  ( 12.50000000000000000, 1.530808498934191521E-15, -10.47749643873921244 ) ) ;
#1878 = ADVANCED_FACE ( 'NONE', ( #2643, #4266 ), #14964, .T. ) ;
#1879 = CARTESIAN_POINT ( 'NONE',  ( 30.42903939560917337, -1.852671564043892660, 5.783357778048667797 ) ) ;
#1880 = EDGE_CURVE ( 'NONE', #12037, #17674, #9682, .T. ) ;
#1881 = CARTESIAN_POINT ( 'NONE',  ( 32.93018312783485158, -2.815471066132994249, -3.627061608673662008 ) ) ;
#1882 = FACE_OUTER_BOUND ( 'NONE', #9076, .T. ) ;
#1883 = CARTESIAN_POINT ( 'NONE',  ( 33.32864623319426300, -4.021405196597508613, 8.283357778048662468 ) ) ;
#1884 = CARTESIAN_POINT ( 'NONE',  ( 30.39102621733566423, -5.629271460726126719, 3.627061608673662896 ) ) ;
#1885 = ORIENTED_EDGE ( 'NONE', *, *, #16260, .F. ) ;
#1886 = CARTESIAN_POINT ( 'NONE',  ( -2.100000000000000089, 2.571758278209441957E-16, 1.159999999999999476 ) ) ;
#1887 = ORIENTED_EDGE ( 'NONE', *, *, #13260, .T. ) ;
#1888 = CARTESIAN_POINT ( 'NONE',  ( 26.45077056032005913, -6.103994453487816330, 3.627061608673662896 ) ) ;
#1889 = CARTESIAN_POINT ( 'NONE',  ( 32.57506351453486815, -6.630276025878011126, -5.113484796970860558 ) ) ;
#1890 = DIRECTION ( 'NONE',  ( 0.000000000000000000, 0.000000000000000000, 1.000000000000000000 ) ) ;
#1891 = ORIENTED_EDGE ( 'NONE', *, *, #9946, .F. ) ;
#1892 = FACE_OUTER_BOUND ( 'NONE', #9347, .T. ) ;
#1893 = PLANE ( 'NONE',  #6940 ) ;
#1894 = CARTESIAN_POINT ( 'NONE',  ( 26.31065902414478330, -7.328232685206446106, 5.254681170202263552 ) ) ;
#1895 = CARTESIAN_POINT ( 'NONE',  ( 26.07857582428556853, -4.894895503279006022, -8.283357778048662468 ) ) ;
#1896 = CARTESIAN_POINT ( 'NONE',  ( 26.15738093914773543, -4.885401043216321959, -8.283357778048662468 ) ) ;
#1897 = CARTESIAN_POINT ( 'NONE',  ( 0.000000000000000000, 0.000000000000000000, -12.00000000000000000 ) ) ;
#1898 = CARTESIAN_POINT ( 'NONE',  ( 38.70301816123731697, -5.700001250565210675, -9.783357778048662468 ) ) ;
#1899 = EDGE_CURVE ( 'NONE', #11176, #14870, #17899, .T. ) ;
#1900 =( NAMED_UNIT ( * ) PLANE_ANGLE_UNIT ( ) SI_UNIT ( $, .RADIAN. ) );
#1901 = CARTESIAN_POINT ( 'NONE',  ( 27.61527553138257574, -4.709753535998224550, -7.939653947423662039 ) ) ;
#1902 = EDGE_LOOP ( 'NONE', ( #17507, #1500, #6103, #12503 ) ) ;
#1903 = CARTESIAN_POINT ( 'NONE',  ( 28.36392410707646761, -4.619556167269785796, 8.283357778048662468 ) ) ;
#1904 = CARTESIAN_POINT ( 'NONE',  ( 33.24613200752366282, -6.212066908601060256, 4.533357778048659803 ) ) ;
#1905 = ADVANCED_FACE ( 'NONE', ( #5430 ), #6623, .T. ) ;
#1906 = B_SPLINE_CURVE_WITH_KNOTS ( 'NONE', 1,
 ( #999, #17710 ),
 .UNSPECIFIED., .F., .F.,
 ( 2, 2 ),
 ( 0.000000000000000000, 1.000000000000000000 ),
 .UNSPECIFIED. ) ;
#1907 = ORIENTED_EDGE ( 'NONE', *, *, #2046, .F. ) ;
#1908 = EDGE_LOOP ( 'NONE', ( #4539, #14023, #8623, #6291 ) ) ;
#1909 = CARTESIAN_POINT ( 'NONE',  ( 26.98483462626008134, -4.785709214840094816, 3.627061608673664228 ) ) ;
#1910 = CARTESIAN_POINT ( 'NONE',  ( 31.66930131758986633, -2.967382423816733894, 7.939653947423662927 ) ) ;
#1911 = CARTESIAN_POINT ( 'NONE',  ( 33.76207435632690590, -3.969185667289998332, -3.627061608673664672 ) ) ;
#1912 = DIRECTION ( 'NONE',  ( 0.6000000000000001998, -0.7999999999999999334, 0.000000000000000000 ) ) ;
#1913 = EDGE_CURVE ( 'NONE', #16642, #16315, #12251, .T. ) ;
#1914 = CARTESIAN_POINT ( 'NONE',  ( -21.62109127008995557, -22.31747812791595464, -15.20678566061929615 ) ) ;
#1916 = EDGE_CURVE ( 'NONE', #2334, #3411, #9512, .T. ) ;
#1915 = CARTESIAN_POINT ( 'NONE',  ( 25.77727992838053339, -5.625024813964539128, -7.939653947423662927 ) ) ;
#1917 = DIRECTION ( 'NONE',  ( -1.000000000000000000, 0.000000000000000000, 0.000000000000000000 ) ) ;
#1918 = CARTESIAN_POINT ( 'NONE',  ( 8.776279441628840772, 6.799038105676637578, -3.000000000000000888 ) ) ;
#1919 = LINE ( 'NONE', #12960, #7002 ) ;
#1920 = PLANE ( 'NONE',  #14245 ) ;
#1921 = PRODUCT_DEFINITION_CONTEXT ( 'detailed design', #1118, 'design' ) ;
#1922 = DIRECTION ( 'NONE',  ( 1.000000000000000000, 0.000000000000000000, 0.000000000000000000 ) ) ;
#1923 = ORIENTED_EDGE ( 'NONE', *, *, #14468, .F. ) ;
#1924 = ORIENTED_EDGE ( 'NONE', *, *, #8512, .F. ) ;
#1925 = CARTESIAN_POINT ( 'NONE',  ( 26.35439372113758694, -4.861664893681965083, -7.939653947423662039 ) ) ;
#1926 = CARTESIAN_POINT ( 'NONE',  ( 0.000000000000000000, 0.000000000000000000, 1.599999999999998979 ) ) ;
#1927 = DIRECTION ( 'NONE',  ( -0.1196152422706621143, 0.9928203230275509661, 0.000000000000000000 ) ) ;
#1928 = DIRECTION ( 'NONE',  ( 0.7999999999999999334, 0.6000000000000001998, -0.000000000000000000 ) ) ;
#1929 = DIRECTION ( 'NONE',  ( -0.000000000000000000, -0.000000000000000000, -1.000000000000000000 ) ) ;
#1930 = ADVANCED_FACE ( 'NONE', ( #16604 ), #9038, .T. ) ;
#1931 = CARTESIAN_POINT ( 'NONE',  ( 27.52714686987067694, -7.627998469090175426, 5.783357778048657138 ) ) ;
#1932 = ORIENTED_EDGE ( 'NONE', *, *, #640, .T. ) ;
#1933 = EDGE_LOOP ( 'NONE', ( #3187, #9440 ) ) ;
#1934 = CYLINDRICAL_SURFACE ( 'NONE', #7061, 2.500000000000001776 ) ;
#1935 = EDGE_LOOP ( 'NONE', ( #10375, #16501, #8325, #11917 ) ) ;
#1936 = ADVANCED_FACE ( 'NONE', ( #10861 ), #2733, .F. ) ;
#1937 = EDGE_CURVE ( 'NONE', #16345, #6066, #10175, .T. ) ;
#1938 = ORIENTED_EDGE ( 'NONE', *, *, #9820, .F. ) ;
#1939 = CARTESIAN_POINT ( 'NONE',  ( 28.28955653359400557, -5.882457056865704637, -3.627061608673668225 ) ) ;
#1940 = CARTESIAN_POINT ( 'NONE',  ( 2.500000000000000000, 2.357898499370432166, -2.385244779468109755E-15 ) ) ;
#1941 = CARTESIAN_POINT ( 'NONE',  ( 27.60205212784272177, -2.830435096530727446, -4.705209693361161349 ) ) ;
#1942 = DIRECTION ( 'NONE',  ( -1.000000000000000000, 0.000000000000000000, 0.000000000000000000 ) ) ;
#1943 = CARTESIAN_POINT ( 'NONE',  ( 33.79776779778399032, -6.145605689821873163, -7.033357778048666908 ) ) ;
#1944 = CARTESIAN_POINT ( 'NONE',  ( 0.000000000000000000, 0.000000000000000000, 0.000000000000000000 ) ) ;
#1945 = CARTESIAN_POINT ( 'NONE',  ( 31.84257795004535652, -2.746633492292519296, -3.283357778048662023 ) ) ;
#1946 = EDGE_CURVE ( 'NONE', #627, #82, #13487, .T. ) ;
#1947 = CYLINDRICAL_SURFACE ( 'NONE', #2819, 2.500000000000001776 ) ;
#1948 = CARTESIAN_POINT ( 'NONE',  ( 31.27962407439061110, -2.387360303286481855, 4.705209693361167567 ) ) ;
#1949 = AXIS2_PLACEMENT_3D ( 'NONE', #7182, #6991, #2648 ) ;
#1950 = ORIENTED_EDGE ( 'NONE', *, *, #13954, .T. ) ;
#1951 = CARTESIAN_POINT ( 'NONE',  ( 30.41656616297672500, -2.191532958677927745, -7.033357778048658027 ) ) ;
#1952 = CARTESIAN_POINT ( 'NONE',  ( -1.917618200156724081E-28, -7.000000000000001776, -17.00000000000000000 ) ) ;
#1953 = CARTESIAN_POINT ( 'NONE',  ( 26.01652455409633902, -4.902371455920926380, 5.783357778048663356 ) ) ;
#1954 = VERTEX_POINT ( 'NONE', #185 ) ;
#1955 = CARTESIAN_POINT ( 'NONE',  ( 5.200000000000002842, 0.000000000000000000, 0.000000000000000000 ) ) ;
#1956 = ORIENTED_EDGE ( 'NONE', *, *, #7800, .T. ) ;
#1957 = CARTESIAN_POINT ( 'NONE',  ( 3.347071143357317702, -15.22052928361023127, -17.00000000000000000 ) ) ;
#1958 = LINE ( 'NONE', #11102, #6988 ) ;
#1959 = CARTESIAN_POINT ( 'NONE',  ( 26.78782184427022983, -4.809445364374452581, -8.283357778048662468 ) ) ;
#1960 = CARTESIAN_POINT ( 'NONE',  ( 29.35841309260160159, -6.680460261459264970, -4.533357778048668685 ) ) ;
#1961 = CARTESIAN_POINT ( 'NONE',  ( -3.248936832696171617, -15.16081378324841111, -17.00000000000000000 ) ) ;
#1962 = DIRECTION ( 'NONE',  ( -5.026720092345836698E-22, 4.581671729415424240E-22, -1.000000000000000000 ) ) ;
#1963 = DIRECTION ( 'NONE',  ( -0.000000000000000000, -0.000000000000000000, 1.000000000000000000 ) ) ;
#1964 = CARTESIAN_POINT ( 'NONE',  ( 27.29063000668916672, -2.568146533142987575, -4.533357778048659803 ) ) ;
#1965 = LINE ( 'NONE', #13109, #4002 ) ;
#1966 = CARTESIAN_POINT ( 'NONE',  ( 33.52375369703867847, -2.544085015380856518, 3.283357778048666464 ) ) ;
#1967 = ORIENTED_EDGE ( 'NONE', *, *, #1296, .F. ) ;
#1968 = B_SPLINE_CURVE_WITH_KNOTS ( 'NONE', 3,
 ( #16333, #16580, #15212, #2528, #8055, #8236, #6868, #6693 ),
 .UNSPECIFIED., .F., .F.,
 ( 4, 2, 2, 4 ),
 ( 0.000000000000000000, 0.002450665683189819262, 0.003675998524784728893, 0.004901331366379638524 ),
 .UNSPECIFIED. ) ;
#1969 = ADVANCED_FACE ( 'NONE', ( #7261 ), #10140, .T. ) ;
#1970 = ORIENTED_EDGE ( 'NONE', *, *, #11657, .T. ) ;
#1971 = CARTESIAN_POINT ( 'NONE',  ( 26.04653150877178902, -5.151432644682725659, 7.991496109485919597 ) ) ;
#1972 = ORIENTED_EDGE ( 'NONE', *, *, #14626, .F. ) ;
#1973 = CARTESIAN_POINT ( 'NONE',  ( 32.82963640218302004, -5.962437625020304388, 6.861505862736157368 ) ) ;
#1974 = CARTESIAN_POINT ( 'NONE',  ( 31.88017671309158274, -6.376637546091784792, -4.533357778048668685 ) ) ;
#1975 = CARTESIAN_POINT ( 'NONE',  ( -4.000000000000000000, -2.309401076758510918, -0.5000000000000000000 ) ) ;
#1976 = ORIENTED_EDGE ( 'NONE', *, *, #6097, .F. ) ;
#1977 = FACE_OUTER_BOUND ( 'NONE', #3480, .T. ) ;
#1978 = ORIENTED_EDGE ( 'NONE', *, *, #804, .F. ) ;
#1979 = CARTESIAN_POINT ( 'NONE',  ( 0.000000000000000000, 0.000000000000000000, 2.399999999999999467 ) ) ;
#1980 = CARTESIAN_POINT ( 'NONE',  ( 32.96626681528915981, -4.065064760026301016, -5.783357778048663356 ) ) ;
#1981 = CARTESIAN_POINT ( 'NONE',  ( 27.10304229683147526, -4.771467524953526329, -3.283357778048664688 ) ) ;
#1982 = VECTOR ( 'NONE', #12816, 1000.000000000000000 ) ;
#1983 = CARTESIAN_POINT ( 'NONE',  ( 28.91480295676398171, -18.24795679052564168, 13.46730161501605316 ) ) ;
#1984 = CARTESIAN_POINT ( 'NONE',  ( 0.000000000000000000, 0.000000000000000000, -2.000000000000000000 ) ) ;
#1985 = CARTESIAN_POINT ( 'NONE',  ( 27.10313151398701947, -6.652368374500619908, -6.861505862736166250 ) ) ;
#1986 = CARTESIAN_POINT ( 'NONE',  ( 25.76775864925888015, -2.837585720338237749, -6.439571894700457655 ) ) ;
#1987 = AXIS2_PLACEMENT_3D ( 'NONE', #1351, #6533, #17634 ) ;
#1988 = CARTESIAN_POINT ( 'NONE',  ( 30.69058026372202974, -5.793053633118939061, 3.283357778048663800 ) ) ;
#1989 = EDGE_CURVE ( 'NONE', #5981, #2327, #463, .T. ) ;
#1990 = ORIENTED_EDGE ( 'NONE', *, *, #11427, .T. ) ;
#1991 = ORIENTED_EDGE ( 'NONE', *, *, #15992, .T. ) ;
#1992 = CIRCLE ( 'NONE', #6018, 2.749999999999988454 ) ;
#1993 = ORIENTED_EDGE ( 'NONE', *, *, #14425, .F. ) ;
#1994 = CARTESIAN_POINT ( 'NONE',  ( 26.45077056032005913, -6.103994453487816330, 3.627061608673662896 ) ) ;
#1995 = CIRCLE ( 'NONE', #508, 2.500000000000000888 ) ;
#1996 = EDGE_CURVE ( 'NONE', #14070, #1615, #10473, .T. ) ;
#1997 = LINE ( 'NONE', #3348, #3999 ) ;
#1998 = FACE_OUTER_BOUND ( 'NONE', #12793, .T. ) ;
#1999 = CARTESIAN_POINT ( 'NONE',  ( -7.511572993685817836E-16, -4.618802153517020059, -4.700000000000000178 ) ) ;
#2000 = CARTESIAN_POINT ( 'NONE',  ( 32.50119254608192421, -4.121097024973739309, -3.627061608673664672 ) ) ;
#2001 = CARTESIAN_POINT ( 'NONE',  ( 30.37154917142620292, -2.923863409590206519, -8.283357778048660691 ) ) ;
#2002 = CARTESIAN_POINT ( 'NONE',  ( 13.60000000000000320, 1.665519646840400618E-15, 0.000000000000000000 ) ) ;
#2003 = CIRCLE ( 'NONE', #14450, 5.384454397937117776 ) ;
#2004 =( BOUNDED_CURVE ( )  B_SPLINE_CURVE ( 2, ( #12224, #6600, #15029, #6524, #5230, #16577, #12036, #9405, #17799 ),
 .UNSPECIFIED., .F., .T. ) 
 B_SPLINE_CURVE_WITH_KNOTS ( ( 3, 2, 2, 2, 3 ),
 ( 0.4423076923076923461, 0.4487179487179487336, 0.4615384615384615641, 0.4743589743589743390, 0.4807692307692307820 ),
 .UNSPECIFIED. ) 
 CURVE ( )  GEOMETRIC_REPRESENTATION_ITEM ( )  RATIONAL_B_SPLINE_CURVE ( ( 0.9330127018922194093, 0.9330127018922196314, 1.000000000000000000, 0.8660254037844387076, 1.000000000000000000, 0.8660254037844387076, 1.000000000000000000, 0.9330127018922190762, 0.9330127018922194093 ) ) 
 REPRESENTATION_ITEM ( '' )  );
#2005 = CARTESIAN_POINT ( 'NONE',  ( -1.393927851585477828, 4.043713361053527855, -3.226374918436836658 ) ) ;
#2006 = CARTESIAN_POINT ( 'NONE',  ( 25.11802603177690330, -16.03270077640482683, -10.53798182577225084 ) ) ;
#2007 = CARTESIAN_POINT ( 'NONE',  ( 30.00264913441657555, -6.940201157507134511, -5.783357778048657138 ) ) ;
#2008 = EDGE_LOOP ( 'NONE', ( #14323, #3119, #13925, #6516, #3343, #3960, #8396, #13583, #9584, #17855, #7809 ) ) ;
#2009 = AXIS2_PLACEMENT_3D ( 'NONE', #10405, #10657, #10838 ) ;
#2010 = CARTESIAN_POINT ( 'NONE',  ( 26.66961417369883591, -4.823687054261037055, -3.627061608673664672 ) ) ;
#2011 = DIRECTION ( 'NONE',  ( 1.000000000000000000, 0.000000000000000000, 0.000000000000000000 ) ) ;
#2012 = VERTEX_POINT ( 'NONE', #11208 ) ;
#2013 = CARTESIAN_POINT ( 'NONE',  ( 2.855764796983343068, -2.970025579236426516, -0.09382832055446284347 ) ) ;
#2014 = CARTESIAN_POINT ( 'NONE',  ( 27.45957062324739795, -6.182326487390973568, 3.283357778048663800 ) ) ;
#2015 = AXIS2_PLACEMENT_3D ( 'NONE', #16835, #9642, #234 ) ;
#2016 = EDGE_LOOP ( 'NONE', ( #5308, #3767, #12168, #12352, #15309 ) ) ;
#2017 = DIRECTION ( 'NONE',  ( -0.9928203230275510771, 0.1196152422706621282, 0.000000000000000000 ) ) ;
#2018 = EDGE_LOOP ( 'NONE', ( #2444, #12565, #15569, #11349, #7141 ) ) ;
#2019 = CARTESIAN_POINT ( 'NONE',  ( 32.67202617590239555, -5.981426544730773287, -4.705209693361168455 ) ) ;
#2020 = VERTEX_POINT ( 'NONE', #15506 ) ;
#2021 = AXIS2_PLACEMENT_3D ( 'NONE', #4297, #4559, #14280 ) ;
#2022 = PLANE ( 'NONE',  #14517 ) ;
#2023 = CARTESIAN_POINT ( 'NONE',  ( 28.74176732417158320, -7.092112515190875044, -5.783357778048657138 ) ) ;
#2024 = ORIENTED_EDGE ( 'NONE', *, *, #16213, .F. ) ;
#2025 = CARTESIAN_POINT ( 'NONE',  ( 27.26074174026764751, -6.633379454790151009, -6.861505862736167138 ) ) ;
#2026 = ADVANCED_FACE ( 'NONE', ( #13966 ), #1920, .F. ) ;
#2027 = CARTESIAN_POINT ( 'NONE',  ( 16.75000000000000000, -16.21813761408365195, -16.03574476417184513 ) ) ;
#2028 = AXIS2_PLACEMENT_3D ( 'NONE', #3780, #17604, #2173 ) ;
#2029 = CARTESIAN_POINT ( 'NONE',  ( 27.73357241910951743, -6.576412695658750529, -6.861505862736166250 ) ) ;
#2030 = DIRECTION ( 'NONE',  ( -1.000000000000000000, 0.000000000000000000, 0.000000000000000000 ) ) ;
#2031 = DIRECTION ( 'NONE',  ( 0.9928203230275510771, 0.1196152422706609902, 4.006172263299092517E-17 ) ) ;
#2032 = CARTESIAN_POINT ( 'NONE',  ( 28.51030546511822195, -6.055733689321201041, -3.283357778048667797 ) ) ;
#2033 = AXIS2_PLACEMENT_3D ( 'NONE', #2874, #15205, #8310 ) ;
#2034 = LINE ( 'NONE', #3299, #16713 ) ;
#2035 = CARTESIAN_POINT ( 'NONE',  ( 31.51621784984448738, -6.120678622607529817, 4.705209693361160461 ) ) ;
#2036 = AXIS2_PLACEMENT_3D ( 'NONE', #500, #8566, #7042 ) ;
#2037 = ORIENTED_EDGE ( 'NONE', *, *, #5868, .T. ) ;
#2038 = CYLINDRICAL_SURFACE ( 'NONE', #14415, 10.50000000000000000 ) ;
#2039 = CARTESIAN_POINT ( 'NONE',  ( 30.71189515440122975, -6.854751018602581958, -5.783357778048663356 ) ) ;
#2040 = DIRECTION ( 'NONE',  ( 1.000000000000000000, 0.000000000000000000, 0.000000000000000000 ) ) ;
#2041 = ORIENTED_EDGE ( 'NONE', *, *, #11253, .F. ) ;
#2042 = DIRECTION ( 'NONE',  ( 0.000000000000000000, 0.000000000000000000, -1.000000000000000000 ) ) ;
#2043 = CIRCLE ( 'NONE', #14497, 3.000000000000000000 ) ;
#2044 = CARTESIAN_POINT ( 'NONE',  ( 25.81704846941310549, -3.246696919197674447, -4.409389677717624245 ) ) ;
#2045 = CARTESIAN_POINT ( 'NONE',  ( 26.01652455409633902, -4.902371455920928156, -5.783357778048663356 ) ) ;
#2046 = EDGE_CURVE ( 'NONE', #11770, #9400, #277, .T. ) ;
#2047 = ORIENTED_EDGE ( 'NONE', *, *, #16346, .F. ) ;
#2048 = CARTESIAN_POINT ( 'NONE',  ( 32.85952466860454280, -1.897204703373130741, 4.533357778048667797 ) ) ;
#2049 = EDGE_CURVE ( 'NONE', #10575, #16479, #17270, .T. ) ;
#2050 = CARTESIAN_POINT ( 'NONE',  ( 28.63031693179632242, -2.406740715396564756, -4.533357778048659803 ) ) ;
#2051 = FACE_OUTER_BOUND ( 'NONE', #14308, .T. ) ;
#2052 = AXIS2_PLACEMENT_3D ( 'NONE', #16004, #7472, #7829 ) ;
#2053 = DIRECTION ( 'NONE',  ( 1.000000000000000000, 0.000000000000000000, 0.000000000000000000 ) ) ;
#2054 = CIRCLE ( 'NONE', #4054, 10.50000000000000000 ) ;
#2055 = ORIENTED_EDGE ( 'NONE', *, *, #15818, .F. ) ;
#2056 =( BOUNDED_CURVE ( )  B_SPLINE_CURVE ( 2, ( #622, #2352, #7871, #13307, #14848, #6512, #15946, #7692, #13401 ),
 .UNSPECIFIED., .F., .T. ) 
 B_SPLINE_CURVE_WITH_KNOTS ( ( 3, 2, 2, 2, 3 ),
 ( 0.9038461538461538547, 0.9102564102564102422, 0.9230769230769231282, 0.9358974358974359031, 0.9423076923076922906 ),
 .UNSPECIFIED. ) 
 CURVE ( )  GEOMETRIC_REPRESENTATION_ITEM ( )  RATIONAL_B_SPLINE_CURVE ( ( 0.9330127018922194093, 0.9330127018922194093, 1.000000000000000000, 0.8660254037844387076, 1.000000000000000000, 0.8660254037844387076, 1.000000000000000000, 0.9330127018922194093, 0.9330127018922194093 ) ) 
 REPRESENTATION_ITEM ( '' )  );
#2057 = CARTESIAN_POINT ( 'NONE',  ( 30.19827253897071273, -3.144612341114420673, -7.939653947423660263 ) ) ;
#2058 = LINE ( 'NONE', #10366, #6162 ) ;
#2059 = DIRECTION ( 'NONE',  ( 0.9928203230275511881, 0.1196152422706614482, 0.000000000000000000 ) ) ;
#2060 = CARTESIAN_POINT ( 'NONE',  ( 27.65911562847151117, -5.958412735707574015, 7.939653947423658487 ) ) ;
#2061 = APPLICATION_CONTEXT ( 'automotive_design' ) ;
#2062 = CIRCLE ( 'NONE', #8124, 3.999999999999998224 ) ;
#2063 = ORIENTED_EDGE ( 'NONE', *, *, #10851, .T. ) ;
#2064 = CARTESIAN_POINT ( 'NONE',  ( 26.66961417369883591, -4.823687054261037055, -3.627061608673664672 ) ) ;
#2065 = ORIENTED_EDGE ( 'NONE', *, *, #5392, .F. ) ;
#2066 = CARTESIAN_POINT ( 'NONE',  ( 32.32618902979206865, -6.650063623909865385, 5.783357778048657138 ) ) ;
#2067 = CARTESIAN_POINT ( 'NONE',  ( -27.54501800341186168, -11.92321325334030568, 13.84074570522889047 ) ) ;
#2068 = CARTESIAN_POINT ( 'NONE',  ( -4.154094228333753414, -2.398367420967510988, -3.421909803043223341 ) ) ;
#2069 = CIRCLE ( 'NONE', #1483, 2.499999999999999556 ) ;
#2070 = VERTEX_POINT ( 'NONE', #1732 ) ;
#2071 = LINE ( 'NONE', #700, #12556 ) ;
#2072 = CYLINDRICAL_SURFACE ( 'NONE', #2603, 2.749999999999992006 ) ;
#2073 = DIRECTION ( 'NONE',  ( 0.9928203230275510771, 0.1196152422706609902, 4.006172263299092517E-17 ) ) ;
#2074 = CARTESIAN_POINT ( 'NONE',  ( 32.28234893270314387, -5.401404424200516807, -7.939653947423664704 ) ) ;
#2076 = ADVANCED_FACE ( 'NONE', ( #5791 ), #16001, .T. ) ;
#2075 = CARTESIAN_POINT ( 'NONE',  ( 27.41826274939272423, -4.733489685532582314, -8.283357778048662468 ) ) ;
#2077 = COLOUR_RGB ( '', 0.08235294, 0.09019608, 0.10196078) ;
#2078 = LINE ( 'NONE', #13396, #17368 ) ;
#2079 = CARTESIAN_POINT ( 'NONE',  ( 0.000000000000000000, 0.000000000000000000, -8.700000000000001066 ) ) ;
#2080 = CARTESIAN_POINT ( 'NONE',  ( 26.66961417369883591, -4.823687054261037055, -3.627061608673664672 ) ) ;
#2081 = SHAPE_REPRESENTATION ( 'o-rings series a_iso_O-ring 19x1.8-A-ISO 3601-1', ( #3575 ), #11602 ) ;
#2082 = EDGE_CURVE ( 'NONE', #6537, #13858, #8523, .T. ) ;
#2083 = DIRECTION ( 'NONE',  ( -1.000000000000000000, 0.000000000000000000, 0.000000000000000000 ) ) ;
#2084 = AXIS2_PLACEMENT_3D ( 'NONE', #8243, #5992, #7288 ) ;
#2085 = CARTESIAN_POINT ( 'NONE',  ( 31.38859741546781379, -7.162769935976271540, 5.783357778048657138 ) ) ;
#2086 = ORIENTED_EDGE ( 'NONE', *, *, #12227, .F. ) ;
#2087 = VERTEX_POINT ( 'NONE', #7361 ) ;
#2088 = CIRCLE ( 'NONE', #6117, 13.00000000000000178 ) ;
#2089 = VERTEX_POINT ( 'NONE', #7177 ) ;
#2090 = DIRECTION ( 'NONE',  ( -0.1196152422706611984, 0.9928203230275510771, 0.000000000000000000 ) ) ;
#2091 = CARTESIAN_POINT ( 'NONE',  ( 31.87075164095941915, -4.197052703815608687, 7.939653947423662039 ) ) ;
#2092 = CARTESIAN_POINT ( 'NONE',  ( 15.92260893619738837, -28.39189527176317540, -16.15082599432113142 ) ) ;
#2093 = CARTESIAN_POINT ( 'NONE',  ( 29.45101334415624095, -7.006662376286321603, -5.783357778048657138 ) ) ;
#2094 = CARTESIAN_POINT ( 'NONE',  ( -17.40358024347774091, -19.00834140588416332, -15.93963985190277910 ) ) ;
#2096 = AXIS2_PLACEMENT_3D ( 'NONE', #4505, #9013, #2405 ) ;
#2095 = CARTESIAN_POINT ( 'NONE',  ( 33.35047706458318828, -2.764833946905071560, -7.939653947423660263 ) ) ;
#2097 = CARTESIAN_POINT ( 'NONE',  ( 2.864813309430322025E-13, -4.796980096169637164, -3.421999068284422130 ) ) ;
#2098 = CARTESIAN_POINT ( 'NONE',  ( -8.632250723006720250, -18.84644399697197770, -13.00000000000000178 ) ) ;
#2099 = CIRCLE ( 'NONE', #13645, 10.50000000000000000 ) ;
#2101 = EDGE_CURVE ( 'NONE', #9766, #6169, #5832, .T. ) ;
#2100 = CARTESIAN_POINT ( 'NONE',  ( 18.99795248260418745, 9.336063356527739998, 15.69100717631305031 ) ) ;
#2102 = DIRECTION ( 'NONE',  ( 0.000000000000000000, -0.5000000000000011102, -0.8660254037844379305 ) ) ;
#2103 =( NAMED_UNIT ( * ) PLANE_ANGLE_UNIT ( ) SI_UNIT ( $, .RADIAN. ) );
#2104 = VERTEX_POINT ( 'NONE', #16884 ) ;
#2105 = ORIENTED_EDGE ( 'NONE', *, *, #8053, .F. ) ;
#2106 = CARTESIAN_POINT ( 'NONE',  ( 25.83772294520678159, -3.669972453104032084, -3.627061608673662896 ) ) ;
#2107 = CARTESIAN_POINT ( 'NONE',  ( 32.08959525433819238, -2.916745304588811205, -7.939653947423660263 ) ) ;
#2108 = VERTEX_POINT ( 'NONE', #10045 ) ;
#2109 = EDGE_CURVE ( 'NONE', #3845, #13908, #12877, .T. ) ;
#2110 = DIRECTION ( 'NONE',  ( 0.000000000000000000, 0.000000000000000000, -1.000000000000000000 ) ) ;
#2111 = CARTESIAN_POINT ( 'NONE',  ( 27.92107091181166467, -2.492190854301117753, 7.033357778048666020 ) ) ;
#2112 = AXIS2_PLACEMENT_3D ( 'NONE', #5664, #8577, #16941 ) ;
#2113 = ORIENTED_EDGE ( 'NONE', *, *, #1989, .T. ) ;
#2114 = CARTESIAN_POINT ( 'NONE',  ( 29.07687923786957285, -2.352938776424351008, -7.033357778048658027 ) ) ;
#2115 = CARTESIAN_POINT ( 'NONE',  ( 30.04066231269008469, -3.163601260824890904, -7.939653947423660263 ) ) ;
#2116 = EDGE_LOOP ( 'NONE', ( #14184, #10060, #9084, #13984 ) ) ;
#2117 = AXIS2_PLACEMENT_3D ( 'NONE', #17022, #2859, #1604 ) ;
#2118 = AXIS2_PLACEMENT_3D ( 'NONE', #9262, #13257, #7651 ) ;
#2119 = CARTESIAN_POINT ( 'NONE',  ( 29.54600080245929306, -4.477139269648729325, -3.283357778048664688 ) ) ;
#2120 = CARTESIAN_POINT ( 'NONE',  ( 28.51030546511822195, -6.055733689321201041, -3.283357778048667797 ) ) ;
#2121 = ORIENTED_EDGE ( 'NONE', *, *, #6696, .F. ) ;
#2122 = EDGE_CURVE ( 'NONE', #11176, #13499, #11590, .T. ) ;
#2123 = CARTESIAN_POINT ( 'NONE',  ( 29.98133424373737199, -5.878503772023492502, -8.283357778048664244 ) ) ;
#2124 = CARTESIAN_POINT ( 'NONE',  ( 27.04606801335823718, -3.524390735323772006, -7.939653947423660263 ) ) ;
#2125 = CIRCLE ( 'NONE', #4141, 10.50000000000000000 ) ;
#2126 = CARTESIAN_POINT ( 'NONE',  ( 25.81099976294218479, -6.186279776075334524, -7.540300355390971987 ) ) ;
#2127 = CARTESIAN_POINT ( 'NONE',  ( 27.84978555093622177, -3.227686124957687586, -8.283357778048660691 ) ) ;
#2128 = CARTESIAN_POINT ( 'NONE',  ( 27.18555652250208610, -2.580805812949960920, -7.033357778048658027 ) ) ;
#2129 = VECTOR ( 'NONE', #4034, 999.9999999999998863 ) ;
#2130 = CARTESIAN_POINT ( 'NONE',  ( 2.756166666307278135, 3.027528586793024612, -2.923144239647247122 ) ) ;
#2131 = CARTESIAN_POINT ( 'NONE',  ( 29.11066736118121057, -3.075774767273946608, -8.283357778048658915 ) ) ;
#2132 = CARTESIAN_POINT ( 'NONE',  ( 28.82057243903374655, -7.082618055128190093, 5.783357778048657138 ) ) ;
#2133 = ADVANCED_FACE ( 'NONE', ( #14241 ), #17160, .F. ) ;
#2134 = AXIS2_PLACEMENT_3D ( 'NONE', #2794, #14951, #12318 ) ;
#2135 = VERTEX_POINT ( 'NONE', #8708 ) ;
#2136 = CARTESIAN_POINT ( 'NONE',  ( 28.53771668024168662, -2.080538600569502794, -5.783357778048658027 ) ) ;
#2137 = CARTESIAN_POINT ( 'NONE',  ( 2.000000000000006217, 3.464101615137751722, -1.401678602859870442E-15 ) ) ;
#2138 = CARTESIAN_POINT ( 'NONE',  ( -2.000000000000005329, -3.464101615137750390, 0.000000000000000000 ) ) ;
#2139 = AXIS2_PLACEMENT_3D ( 'NONE', #14071, #4278, #15607 ) ;
#2140 = ORIENTED_EDGE ( 'NONE', *, *, #5392, .T. ) ;
#2141 = CARTESIAN_POINT ( 'NONE',  ( 0.000000000000000000, 0.000000000000000000, -3.000000000000002665 ) ) ;
#2142 = FACE_BOUND ( 'NONE', #15014, .T. ) ;
#2143 = CARTESIAN_POINT ( 'NONE',  ( 25.80685721358263152, -3.162108319002908896, -4.519686641326834398 ) ) ;
#2144 = CARTESIAN_POINT ( 'NONE',  ( 32.82963640218302004, -5.962437625020304388, -4.705209693361169343 ) ) ;
#2145 = LINE ( 'NONE', #2321, #7341 ) ;
#2146 = EDGE_CURVE ( 'NONE', #9766, #2089, #1830, .T. ) ;
#2147 = ORIENTED_EDGE ( 'NONE', *, *, #8896, .T. ) ;
#2148 = CARTESIAN_POINT ( 'NONE',  ( 28.09753128235661279, -6.832371619143005503, -4.533357778048668685 ) ) ;
#2149 = DIRECTION ( 'NONE',  ( 0.9928203230275512992, 0.1196152422706614482, 0.000000000000000000 ) ) ;
#2150 = FACE_OUTER_BOUND ( 'NONE', #10317, .T. ) ;
#2151 = CARTESIAN_POINT ( 'NONE',  ( 30.17635249042624679, -2.520282741259753045, -6.861505862736158257 ) ) ;
#2152 = VECTOR ( 'NONE', #543, 1000.000000000000000 ) ;
#2153 = DIRECTION ( 'NONE',  ( -0.1196152422706609625, 0.9928203230275510771, 0.000000000000000000 ) ) ;
#2154 = CARTESIAN_POINT ( 'NONE',  ( 2.100000000000000089, 0.000000000000000000, -4.394516984716110741 ) ) ;
#2155 = MECHANICAL_DESIGN_GEOMETRIC_PRESENTATION_REPRESENTATION (  '', ( #11365 ), #3597 ) ;
#2156 = CARTESIAN_POINT ( 'NONE',  ( 27.77288575766320378, -4.690764616287755651, 3.627061608673664228 ) ) ;
#2157 = EDGE_CURVE ( 'NONE', #692, #13923, #12313, .T. ) ;
#2158 = ORIENTED_EDGE ( 'NONE', *, *, #11848, .F. ) ;
#2159 = CARTESIAN_POINT ( 'NONE',  ( 26.98483462626008134, -4.785709214840094816, -7.939653947423662039 ) ) ;
#2160 = VERTEX_POINT ( 'NONE', #13053 ) ;
#2161 = CARTESIAN_POINT ( 'NONE',  ( 33.13163345120441505, -4.045141346131868154, 7.939653947423662039 ) ) ;
#2162 = CARTESIAN_POINT ( 'NONE',  ( -20.46503100693326260, -10.50166121531458430, 15.42720773483998009 ) ) ;
#2163 = CARTESIAN_POINT ( 'NONE',  ( 27.50903986916043920, -7.240631829073577386, -6.453230759126468818 ) ) ;
#2164 = ORIENTED_EDGE ( 'NONE', *, *, #6228, .F. ) ;
#2165 = DIRECTION ( 'NONE',  ( -1.000000000000000000, 0.000000000000000000, 0.000000000000000000 ) ) ;
#2166 = CARTESIAN_POINT ( 'NONE',  ( 25.95642634701329499, -4.403549397486667516, -3.686412874245489135 ) ) ;
#2167 = FACE_OUTER_BOUND ( 'NONE', #2291, .T. ) ;
#2168 = EDGE_CURVE ( 'NONE', #15348, #7502, #4785, .T. ) ;
#2169 = CARTESIAN_POINT ( 'NONE',  ( 32.50119254608192421, -4.121097024973739309, -3.627061608673664672 ) ) ;
#2170 =( BOUNDED_CURVE ( )  B_SPLINE_CURVE ( 2, ( #3547, #12323, #8596, #16419, #8158, #5418, #12405, #11027, #9671 ),
 .UNSPECIFIED., .F., .T. ) 
 B_SPLINE_CURVE_WITH_KNOTS ( ( 3, 2, 2, 2, 3 ),
 ( 0.2500000000000000000, 0.2564102564102563875, 0.2692307692307692180, 0.2820512820512820484, 0.2884615384615384914 ),
 .UNSPECIFIED. ) 
 CURVE ( )  GEOMETRIC_REPRESENTATION_ITEM ( )  RATIONAL_B_SPLINE_CURVE ( ( 0.9330127018922194093, 0.9330127018922195203, 1.000000000000000000, 0.8660254037844387076, 1.000000000000000000, 0.8660254037844387076, 1.000000000000000000, 0.9330127018922190762, 0.9330127018922194093 ) ) 
 REPRESENTATION_ITEM ( '' )  );
#2171 = CARTESIAN_POINT ( 'NONE',  ( 32.56242593318007295, -2.859778545457410281, -7.939653947423660263 ) ) ;
#2172 = CYLINDRICAL_SURFACE ( 'NONE', #7782, 6.000000000000000888 ) ;
#2173 = DIRECTION ( 'NONE',  ( 0.000000000000000000, 0.000000000000000000, 1.000000000000000000 ) ) ;
#2174 = CARTESIAN_POINT ( 'NONE',  ( 27.72904566057427189, -3.442105416578422172, -3.627061608673662896 ) ) ;
#2175 = CARTESIAN_POINT ( 'NONE',  ( 31.61111609099199171, -1.710254666422835745, -5.783357778048662468 ) ) ;
#2176 = CARTESIAN_POINT ( 'NONE',  ( 31.64365984991007252, -1.316785610144591390, 5.783357778048668685 ) ) ;
#2177 = ORIENTED_EDGE ( 'NONE', *, *, #13897, .T. ) ;
#2178 = ADVANCED_FACE ( 'NONE', ( #14695 ), #15693, .T. ) ;
#2179 = VERTEX_POINT ( 'NONE', #6341 ) ;
#2180 = ORIENTED_EDGE ( 'NONE', *, *, #6084, .T. ) ;
#2181 = B_SPLINE_CURVE_WITH_KNOTS ( 'NONE', 3,
 ( #758, #8747, #3477, #11437, #8919, #4651 ),
 .UNSPECIFIED., .F., .F.,
 ( 4, 2, 4 ),
 ( -3.640115492409826693E-06, 0.0002066546034006530282, 0.0004169493222937159212 ),
 .UNSPECIFIED. ) ;
#2182 = FACE_OUTER_BOUND ( 'NONE', #17259, .T. ) ;
#2183 = CARTESIAN_POINT ( 'NONE',  ( -9.099998387031003944, -19.29508120620799616, -16.81964500401478091 ) ) ;
#2184 = DIRECTION ( 'NONE',  ( -0.000000000000000000, -0.000000000000000000, -1.000000000000000000 ) ) ;
#2185 = CARTESIAN_POINT ( 'NONE',  ( -45.50000000000000000, -19.03270077640483038, -8.287981825772241962 ) ) ;
#2186 = FACE_OUTER_BOUND ( 'NONE', #6238, .T. ) ;
#2187 = CARTESIAN_POINT ( 'NONE',  ( 29.66420847303068697, -4.462897579762144851, -7.939653947423662039 ) ) ;
#2188 = CARTESIAN_POINT ( 'NONE',  ( 29.11066736118121767, -3.075774767273946608, 3.283357778048666464 ) ) ;
#2189 = EDGE_CURVE ( 'NONE', #3360, #2203, #14783, .T. ) ;
#2190 = LINE ( 'NONE', #7621, #15372 ) ;
#2191 = CARTESIAN_POINT ( 'NONE',  ( 33.00219691583784964, -5.514549477365426888, -3.283357778048667797 ) ) ;
#2192 = CARTESIAN_POINT ( 'NONE',  ( 34.07870238058739432, -4.938269840783200415, 5.783357778048663356 ) ) ;
#2193 =( BOUNDED_CURVE ( )  B_SPLINE_CURVE ( 2, ( #3270, #15780, #8802, #14334, #11589, #3355, #8887, #5320, #13505 ),
 .UNSPECIFIED., .F., .T. ) 
 B_SPLINE_CURVE_WITH_KNOTS ( ( 3, 2, 2, 2, 3 ),
 ( 0.5192307692307692735, 0.5256410256410256610, 0.5384615384615384359, 0.5512820512820513219, 0.5576923076923077094 ),
 .UNSPECIFIED. ) 
 CURVE ( )  GEOMETRIC_REPRESENTATION_ITEM ( )  RATIONAL_B_SPLINE_CURVE ( ( 0.9330127018922192983, 0.9330127018922198534, 1.000000000000000000, 0.8660254037844387076, 1.000000000000000000, 0.8660254037844387076, 1.000000000000000000, 0.9330127018922194093, 0.9330127018922194093 ) ) 
 REPRESENTATION_ITEM ( '' )  );
#2194 = FACE_OUTER_BOUND ( 'NONE', #12338, .T. ) ;
#2195 =( NAMED_UNIT ( * ) PLANE_ANGLE_UNIT ( ) SI_UNIT ( $, .RADIAN. ) );
#2196 = EDGE_LOOP ( 'NONE', ( #15610, #7635, #5937, #16842 ) ) ;
#2197 = CARTESIAN_POINT ( 'NONE',  ( 26.24062359194589078, -6.129313013101781671, -3.627061608673667781 ) ) ;
#2198 = CARTESIAN_POINT ( 'NONE',  ( 31.44176105920648112, -5.502678662656354192, -3.627061608673668225 ) ) ;
#2199 = ORIENTED_EDGE ( 'NONE', *, *, #1098, .T. ) ;
#2200 = DIRECTION ( 'NONE',  ( 0.000000000000000000, 0.000000000000000000, 1.000000000000000000 ) ) ;
#2201 = CARTESIAN_POINT ( 'NONE',  ( 33.95908713831673964, -3.945449517755641455, 8.283357778048662468 ) ) ;
#2202 = EDGE_CURVE ( 'NONE', #9429, #14403, #16502, .T. ) ;
#2203 = VERTEX_POINT ( 'NONE', #17344 ) ;
#2204 = FACE_OUTER_BOUND ( 'NONE', #7802, .T. ) ;
#2205 = CARTESIAN_POINT ( 'NONE',  ( 31.38469755857769528, -2.374701023479507178, -4.705209693361161349 ) ) ;
#2206 = ORIENTED_EDGE ( 'NONE', *, *, #3217, .T. ) ;
#2207 = DIRECTION ( 'NONE',  ( 0.000000000000000000, 0.000000000000000000, -1.000000000000000000 ) ) ;
#2208 = CARTESIAN_POINT ( 'NONE',  ( 26.03655646321512052, -5.068638614726478586, -8.187879365734106685 ) ) ;
#2209 = EDGE_CURVE ( 'NONE', #17076, #8205, #13389, .T. ) ;
#2210 = CARTESIAN_POINT ( 'NONE',  ( 0.000000000000000000, 0.000000000000000000, 12.00000000000000000 ) ) ;
#2211 = AXIS2_PLACEMENT_3D ( 'NONE', #2686, #8215, #6764 ) ;
#2212 = CARTESIAN_POINT ( 'NONE',  ( 31.00199007654869732, -2.847907730748336252, -8.283357778048658915 ) ) ;
#2213 = VERTEX_POINT ( 'NONE', #904 ) ;
#2214 = CARTESIAN_POINT ( 'NONE',  ( 26.88845778707760914, -3.543379655034240905, -7.939653947423660263 ) ) ;
#2215 = CARTESIAN_POINT ( 'NONE',  ( 26.11428532722776197, -5.713797161519015511, -3.668609639089262409 ) ) ;
#2216 = CARTESIAN_POINT ( 'NONE',  ( 32.37175601071535169, -5.590505156207296267, -3.283357778048667797 ) ) ;
#2217 = CARTESIAN_POINT ( 'NONE',  ( 3.472352378023213504, 2.614038573344063199, -3.020318136128407271 ) ) ;
#2218 = CARTESIAN_POINT ( 'NONE',  ( 29.41846958523816724, -7.400131432564565515, -5.783357778048669573 ) ) ;
#2219 = CARTESIAN_POINT ( 'NONE',  ( 31.88814493096864311, -1.687075024589942407, -5.783357778048658915 ) ) ;
#2220 = EDGE_CURVE ( 'NONE', #15040, #7588, #15871, .T. ) ;
#2221 = EDGE_LOOP ( 'NONE', ( #4763, #5855, #16871, #3173 ) ) ;
#2222 = CARTESIAN_POINT ( 'NONE',  ( 33.95908713831673964, -3.945449517755641455, 8.283357778048662468 ) ) ;
#2223 = CARTESIAN_POINT ( 'NONE',  ( 26.64639396487419987, -2.308405637095112706, -5.783357778048658027 ) ) ;
#2224 = DIRECTION ( 'NONE',  ( 0.000000000000000000, 0.000000000000000000, 1.000000000000000000 ) ) ;
#2225 = EDGE_CURVE ( 'NONE', #7023, #8221, #11865, .T. ) ;
#2226 = VERTEX_POINT ( 'NONE', #13147 ) ;
#2227 = CARTESIAN_POINT ( 'NONE',  ( -25.11802603177690330, -19.03270077640483038, 0.5379818257722508434 ) ) ;
#2228 = CARTESIAN_POINT ( 'NONE',  ( 25.89388370423996832, -3.884438240559767053, -3.881334880282079514 ) ) ;
#2229 = DIRECTION ( 'NONE',  ( 0.000000000000000000, 0.000000000000000000, 1.000000000000000000 ) ) ;
#2230 = DIRECTION ( 'NONE',  ( 5.026720092345836698E-22, -4.581671729415424240E-22, 1.000000000000000000 ) ) ;
#2231 = EDGE_CURVE ( 'NONE', #15452, #4832, #62, .T. ) ;
#2232 = CARTESIAN_POINT ( 'NONE',  ( 30.12771560522282499, -7.314681293660012074, -5.783357778048669573 ) ) ;
#2233 = FACE_OUTER_BOUND ( 'NONE', #13086, .T. ) ;
#2234 = ITEM_DEFINED_TRANSFORMATION ( 'NONE', 'NONE', #3899,  #3575 ) ;
#2235 = DIRECTION ( 'NONE',  ( 1.000000000000000000, 0.000000000000000000, 0.000000000000000000 ) ) ;
#2236 = DIRECTION ( 'NONE',  ( 0.9928203230275512992, 0.1196152422706614898, -0.000000000000000000 ) ) ;
#2237 = CARTESIAN_POINT ( 'NONE',  ( 31.44176105920648823, -5.502678662656354192, -3.627061608673668225 ) ) ;
#2238 = CARTESIAN_POINT ( 'NONE',  ( 8.472608240843633681E-22, -7.722472891792491889E-22, -7.794427190999915211 ) ) ;
#2239 = CARTESIAN_POINT ( 'NONE',  ( 26.07857582428556853, -4.894895503279006022, -8.283357778048662468 ) ) ;
#2240 = CARTESIAN_POINT ( 'NONE',  ( 26.82722439997946395, -4.804698134550569044, 7.939653947423662039 ) ) ;
#2241 = ORIENTED_EDGE ( 'NONE', *, *, #2202, .T. ) ;
#2242 = ORIENTED_EDGE ( 'NONE', *, *, #608, .T. ) ;
#2243 = ORIENTED_EDGE ( 'NONE', *, *, #6742, .F. ) ;
#2244 = CARTESIAN_POINT ( 'NONE',  ( 26.49461065740898036, -7.352653653197164019, 5.783357778048658027 ) ) ;
#2245 =( NAMED_UNIT ( * ) PLANE_ANGLE_UNIT ( ) SI_UNIT ( $, .RADIAN. ) );
#2246 = CARTESIAN_POINT ( 'NONE',  ( -3.679171394226034231, -2.494631558665840299, -0.3503314178412554880 ) ) ;
#2247 = VERTEX_POINT ( 'NONE', #2192 ) ;
#2248 = CARTESIAN_POINT ( 'NONE',  ( 0.000000000000000000, 0.000000000000000000, -3.000000000000002665 ) ) ;
#2249 = CARTESIAN_POINT ( 'NONE',  ( 30.49166216014303643, -4.363205751385915931, 3.283357778048664244 ) ) ;
#2250 = CARTESIAN_POINT ( 'NONE',  ( 10.27627944162880702, -4.200961894323389956, -11.72793873352923910 ) ) ;
#2251 = CARTESIAN_POINT ( 'NONE',  ( 32.06767520579373354, -2.292415704734142690, -6.861505862736158257 ) ) ;
#2252 = CARTESIAN_POINT ( 'NONE',  ( 32.51858583609114106, -1.611119345748072362, -5.783357778048658027 ) ) ;
#2253 = EDGE_CURVE ( 'NONE', #1497, #8671, #17443, .T. ) ;
#2254 = CARTESIAN_POINT ( 'NONE',  ( -1.360615521533533379, 4.061278559078136396, -3.205052026701836532 ) ) ;
#2255 = CARTESIAN_POINT ( 'NONE',  ( 31.95146207396702565, -5.641142275435199416, -8.283357778048664244 ) ) ;
#2256 = CARTESIAN_POINT ( 'NONE',  ( 27.62849893492243325, -6.589071975465733644, -4.705209693361168455 ) ) ;
#2257 = AXIS2_PLACEMENT_3D ( 'NONE', #15530, #4553, #404 ) ;
#2258 = CARTESIAN_POINT ( 'NONE',  ( 26.82912971812489644, -6.258282166232842947, -8.283357778048664244 ) ) ;
#2259 = FACE_OUTER_BOUND ( 'NONE', #1681, .T. ) ;
#2260 = DIRECTION ( 'NONE',  ( 0.000000000000000000, 0.000000000000000000, 1.000000000000000000 ) ) ;
#2261 = CARTESIAN_POINT ( 'NONE',  ( 31.11087420047036289, -5.742416513891037688, 8.283357778048658915 ) ) ;
#2262 = EDGE_CURVE ( 'NONE', #7372, #496, #3710, .T. ) ;
#2263 = VERTEX_POINT ( 'NONE', #4975 ) ;
#2264 = EDGE_LOOP ( 'NONE', ( #291, #15770, #3880, #3682, #12528, #12381 ) ) ;
#2265 = VERTEX_POINT ( 'NONE', #9233 ) ;
#2266 = CARTESIAN_POINT ( 'NONE',  ( 26.21417678486618641, -2.370676134166772808, 5.783357778048668685 ) ) ;
#2267 = CARTESIAN_POINT ( 'NONE',  ( 32.07220196432898263, -5.426722983814484813, 7.939653947423658487 ) ) ;
#2268 = ORIENTED_EDGE ( 'NONE', *, *, #8081, .F. ) ;
#2269 =( BOUNDED_CURVE ( )  B_SPLINE_CURVE ( 2, ( #214, #5722, #11240, #16816, #4817, #7292, #5816, #11525, #10259 ),
 .UNSPECIFIED., .F., .T. ) 
 B_SPLINE_CURVE_WITH_KNOTS ( ( 3, 2, 2, 2, 3 ),
 ( 0.2500000000000000000, 0.2564102564102563875, 0.2692307692307692180, 0.2820512820512820484, 0.2884615384615384914 ),
 .UNSPECIFIED. ) 
 CURVE ( )  GEOMETRIC_REPRESENTATION_ITEM ( )  RATIONAL_B_SPLINE_CURVE ( ( 0.9330127018922194093, 0.9330127018922195203, 1.000000000000000000, 0.8660254037844387076, 1.000000000000000000, 0.8660254037844387076, 1.000000000000000000, 0.9330127018922190762, 0.9330127018922194093 ) ) 
 REPRESENTATION_ITEM ( '' )  );
#2270 = AXIS2_PLACEMENT_3D ( 'NONE', #16996, #14080, #1666 ) ;
#2271 = DIRECTION ( 'NONE',  ( 1.000000000000000000, 0.000000000000000000, 0.000000000000000000 ) ) ;
#2272 = LINE ( 'NONE', #9403, #6139 ) ;
#2273 = CARTESIAN_POINT ( 'NONE',  ( 29.52399153675929355, -1.971908820246954130, -5.783357778048658027 ) ) ;
#2274 = CARTESIAN_POINT ( 'NONE',  ( 33.04340326765378677, -1.875050963503474222, -4.533357778048659803 ) ) ;
#2275 = CARTESIAN_POINT ( 'NONE',  ( 8.409399735147211686E-16, 4.618802153517009401, -4.700000000000000178 ) ) ;
#2276 = CARTESIAN_POINT ( 'NONE',  ( 32.41296236253129592, -1.951006642345344044, -4.533357778048659803 ) ) ;
#2277 = EDGE_CURVE ( 'NONE', #10674, #16241, #17626, .T. ) ;
#2278 = CARTESIAN_POINT ( 'NONE',  ( 46.70046462172870605, -5.135117178011730843, -5.783357778048661579 ) ) ;
#2279 = ADVANCED_FACE ( 'NONE', ( #3634, #14422 ), #9157, .T. ) ;
#2280 = FILL_AREA_STYLE ('',( #9238 ) ) ;
#2281 = CARTESIAN_POINT ( 'NONE',  ( 31.44176105920648823, -5.502678662656354192, -3.627061608673668225 ) ) ;
#2282 = CARTESIAN_POINT ( 'NONE',  ( 30.92509028327567933, -4.310986222078405206, -7.939653947423662039 ) ) ;
#2283 = ORIENTED_EDGE ( 'NONE', *, *, #13061, .T. ) ;
#2284 = CARTESIAN_POINT ( 'NONE',  ( 0.000000000000000000, 0.000000000000000000, 0.000000000000000000 ) ) ;
#2285 = MECHANICAL_DESIGN_GEOMETRIC_PRESENTATION_REPRESENTATION (  '', ( #17928 ), #1396 ) ;
#2286 = CARTESIAN_POINT ( 'NONE',  ( 26.07857582428556853, -4.894895503279006022, 3.283357778048664244 ) ) ;
#2287 = VECTOR ( 'NONE', #16653, 1000.000000000000000 ) ;
#2288 = ORIENTED_EDGE ( 'NONE', *, *, #17671, .F. ) ;
#2289 = CARTESIAN_POINT ( 'NONE',  ( 33.14105852333657509, -6.224726188408045147, -4.533357778048668685 ) ) ;
#2290 = CARTESIAN_POINT ( 'NONE',  ( 32.77257290155422709, -2.834459985843462260, -3.627061608673662896 ) ) ;
#2291 = EDGE_LOOP ( 'NONE', ( #13405, #6679, #1165, #2943, #17413 ) ) ;
#2292 =( BOUNDED_CURVE ( )  B_SPLINE_CURVE ( 3, ( #631, #4611, #13141, #459 ),
 .UNSPECIFIED., .F., .T. ) 
 B_SPLINE_CURVE_WITH_KNOTS ( ( 4, 4 ),
 ( 1.316154292592045083, 1.436990331221392081 ),
 .UNSPECIFIED. ) 
 CURVE ( )  GEOMETRIC_REPRESENTATION_ITEM ( )  RATIONAL_B_SPLINE_CURVE ( ( 1.000000000000000000, 0.9987835910734581546, 0.9987835910734581546, 1.000000000000000000 ) ) 
 REPRESENTATION_ITEM ( '' )  );
#2293 = FACE_OUTER_BOUND ( 'NONE', #16616, .T. ) ;
#2294 = CARTESIAN_POINT ( 'NONE',  ( 27.82847066025702887, -2.165988739474055791, -5.783357778048658027 ) ) ;
#2295 = CARTESIAN_POINT ( 'NONE',  ( 25.78902048130849423, -3.014061381488923885, 6.808963882184758454 ) ) ;
#2296 = B_SPLINE_CURVE_WITH_KNOTS ( 'NONE', 1,
 ( #16667, #17795 ),
 .UNSPECIFIED., .F., .F.,
 ( 2, 2 ),
 ( 0.000000000000000000, 1.000000000000000000 ),
 .UNSPECIFIED. ) ;
#2297 = AXIS2_PLACEMENT_3D ( 'NONE', #11180, #16751, #15385 ) ;
#2298 = DIRECTION ( 'NONE',  ( -1.000000000000000000, 0.000000000000000000, 0.000000000000000000 ) ) ;
#2299 = CARTESIAN_POINT ( 'NONE',  ( 32.22908376348204484, -1.973160382215000785, -7.033357778048658027 ) ) ;
#2300 =( REPRESENTATION_RELATIONSHIP ('NONE','NONE', #3227, #1480 ) REPRESENTATION_RELATIONSHIP_WITH_TRANSFORMATION ( #6389 )SHAPE_REPRESENTATION_RELATIONSHIP( ) );
#2301 = EDGE_CURVE ( 'NONE', #2020, #7100, #4116, .T. ) ;
#2302 = CARTESIAN_POINT ( 'NONE',  ( 28.13194630731337753, -5.901445976576171759, -3.627061608673667781 ) ) ;
#2303 = CARTESIAN_POINT ( 'NONE',  ( 25.71748644841968456, -2.420320648352046078, -5.783357778048663356 ) ) ;
#2304 = DIRECTION ( 'NONE',  ( 0.9928203230275510771, 0.1196152422706609902, 4.006172263299092517E-17 ) ) ;
#2305 = CARTESIAN_POINT ( 'NONE',  ( -23.00000000000000000, -16.21813761408365195, 13.00000000000000178 ) ) ;
#2306 = CARTESIAN_POINT ( 'NONE',  ( 27.33945763453056088, -4.742984145595265488, -8.283357778048662468 ) ) ;
#2307 = CARTESIAN_POINT ( 'NONE',  ( 31.51169109130924184, -2.986371343527201905, -3.627061608673662896 ) ) ;
#2308 = ADVANCED_FACE ( 'NONE', ( #1344 ), #13506, .T. ) ;
#2309 = CIRCLE ( 'NONE', #4601, 10.50000000000000000 ) ;
#2310 = ORIENTED_EDGE ( 'NONE', *, *, #11089, .T. ) ;
#2311 = ORIENTED_EDGE ( 'NONE', *, *, #16894, .F. ) ;
#2312 = DIRECTION ( 'NONE',  ( 0.000000000000000000, 0.000000000000000000, 1.000000000000000000 ) ) ;
#2313 = CARTESIAN_POINT ( 'NONE',  ( -19.71718888926883650, -28.93397812220196030, -15.64003640126278682 ) ) ;
#2314 = ORIENTED_EDGE ( 'NONE', *, *, #5721, .T. ) ;
#2315 = CARTESIAN_POINT ( 'NONE',  ( 25.76466184735054910, -2.811881907026620553, 5.318565573966401061 ) ) ;
#2316 = TOROIDAL_SURFACE ( 'NONE', #17676, 12.70000000000000284, 0.9000000000000003553 ) ;
#2317 = PRODUCT ( 'socket head cap screw_iso_ISO 4762 M5 x 35 - 22N', 'socket head cap screw_iso_ISO 4762 M5 x 35 - 22N', '', ( #5743 ) ) ;
#2318 = DIRECTION ( 'NONE',  ( -1.000000000000000000, 0.000000000000000000, 0.000000000000000000 ) ) ;
#2319 = DIRECTION ( 'NONE',  ( 1.000000000000000000, 4.440892098500626951E-15, 0.000000000000000000 ) ) ;
#2320 = ORIENTED_EDGE ( 'NONE', *, *, #17453, .T. ) ;
#2321 = CARTESIAN_POINT ( 'NONE',  ( -45.00000000000000711, -16.03270077640482683, -0.5379818257722508434 ) ) ;
#2322 = AXIS2_PLACEMENT_3D ( 'NONE', #6054, #3437, #5876 ) ;
#2323 = ADVANCED_FACE ( 'NONE', ( #2619 ), #6958, .F. ) ;
#2324 = CARTESIAN_POINT ( 'NONE',  ( 27.53837573810956130, -6.172832027328289506, -8.283357778048662468 ) ) ;
#2325 = CARTESIAN_POINT ( 'NONE',  ( -3.538288549924106796, -15.34800872113743431, -16.99955934415556769 ) ) ;
#2326 = CARTESIAN_POINT ( 'NONE',  ( 31.58296173575813981, -1.713646710223874381, 5.113484796970860558 ) ) ;
#2327 = VERTEX_POINT ( 'NONE', #1435 ) ;
#2328 = CARTESIAN_POINT ( 'NONE',  ( 30.82871344409320713, -3.068656662272551738, -7.939653947423660263 ) ) ;
#2329 = DIRECTION ( 'NONE',  ( 1.000000000000000000, 0.000000000000000000, 0.000000000000000000 ) ) ;
#2330 = DIRECTION ( 'NONE',  ( 0.000000000000000000, 0.000000000000000000, -1.000000000000000000 ) ) ;
#2331 = CARTESIAN_POINT ( 'NONE',  ( 26.63030083514515312, -6.709335133632020387, 4.705209693361159573 ) ) ;
#2332 = CIRCLE ( 'NONE', #11565, 3.000000000000001332 ) ;
#2333 = ADVANCED_FACE ( 'NONE', ( #3809 ), #12134, .F. ) ;
#2334 = VERTEX_POINT ( 'NONE', #10754 ) ;
#2335 = AXIS2_PLACEMENT_3D ( 'NONE', #8561, #1680, #16923 ) ;
#2336 = CARTESIAN_POINT ( 'NONE',  ( 30.28142597461332741, -2.507623461452779701, 6.861505862736166250 ) ) ;
#2337 = CARTESIAN_POINT ( 'NONE',  ( -28.60529878918911706, -13.42304697295875648, 13.55371198823188017 ) ) ;
#2338 = CARTESIAN_POINT ( 'NONE',  ( 0.000000000000000000, 0.000000000000000000, -4.000000000000000000 ) ) ;
#2339 = ORIENTED_EDGE ( 'NONE', *, *, #4394, .T. ) ;
#2340 = SURFACE_STYLE_FILL_AREA ( #17513 ) ;
#2341 = DIRECTION ( 'NONE',  ( 0.6000000000000000888, -0.7999999999999999334, 0.000000000000000000 ) ) ;
#2342 = ORIENTED_EDGE ( 'NONE', *, *, #11382, .F. ) ;
#2343 = DIRECTION ( 'NONE',  ( 0.5000000000000038858, 0.8660254037844363761, 0.000000000000000000 ) ) ;
#2344 = CARTESIAN_POINT ( 'NONE',  ( 33.76207435632690590, -3.969185667289998332, -3.627061608673664672 ) ) ;
#2345 = CARTESIAN_POINT ( 'NONE',  ( 31.49429780130001433, -5.496349022752856861, -7.939653947423664704 ) ) ;
#2346 = DIRECTION ( 'NONE',  ( -1.000000000000000000, 0.000000000000000000, 0.000000000000000000 ) ) ;
#2347 = CARTESIAN_POINT ( 'NONE',  ( 33.95908713831673964, -3.945449517755637903, -5.783357778048663356 ) ) ;
#2348 = CARTESIAN_POINT ( 'NONE',  ( 30.09392748191118017, -6.591845302810410701, -7.033357778048666908 ) ) ;
#2349 = AXIS2_PLACEMENT_3D ( 'NONE', #9861, #374, #7085 ) ;
#2350 = CARTESIAN_POINT ( 'NONE',  ( 3.538288549924106796, -15.34800872113743431, 16.99955934415557479 ) ) ;
#2351 = CARTESIAN_POINT ( 'NONE',  ( -23.00000000000000000, -16.21813761408365195, 0.000000000000000000 ) ) ;
#2352 = CARTESIAN_POINT ( 'NONE',  ( 26.82229025357024454, -7.323371595517525812, -5.113484796970862334 ) ) ;
#2353 = CARTESIAN_POINT ( 'NONE',  ( 29.21955148510287614, -5.970283550416647600, 8.283357778048658915 ) ) ;
#2354 = AXIS2_PLACEMENT_3D ( 'NONE', #15166, #4012, #1213 ) ;
#2355 = ORIENTED_EDGE ( 'NONE', *, *, #14140, .F. ) ;
#2356 = ORIENTED_EDGE ( 'NONE', *, *, #12370, .T. ) ;
#2357 = EDGE_LOOP ( 'NONE', ( #15581, #5028, #8207, #8002 ) ) ;
#2358 = ADVANCED_FACE ( 'NONE', ( #8315 ), #3253, .T. ) ;
#2359 = CARTESIAN_POINT ( 'NONE',  ( 30.78070346053490880, -6.209293581256383199, 6.861505862736158257 ) ) ;
#2360 = CARTESIAN_POINT ( 'NONE',  ( 28.28502977505876359, -2.748149777785362957, 4.705209693361168455 ) ) ;
#2361 = ORIENTED_EDGE ( 'NONE', *, *, #11040, .F. ) ;
#2362 = CARTESIAN_POINT ( 'NONE',  ( 2.749999999999988454, -20.49999999999999645, 13.00000000000000355 ) ) ;
#2363 = CIRCLE ( 'NONE', #5819, 2.749999999999992895 ) ;
#2364 = DIRECTION ( 'NONE',  ( 0.7999999999999999334, 0.6000000000000001998, 0.000000000000000000 ) ) ;
#2365 = MECHANICAL_DESIGN_GEOMETRIC_PRESENTATION_REPRESENTATION (  '', ( #17736 ), #15665 ) ;
#2366 = CARTESIAN_POINT ( 'NONE',  ( -2.016448651773435938E-27, -20.49999999999999645, -6.000000000000000000 ) ) ;
#2367 = CARTESIAN_POINT ( 'NONE',  ( 30.17635249042624679, -2.520282741259753045, -6.861505862736158257 ) ) ;
#2368 = CARTESIAN_POINT ( 'NONE',  ( 28.53771668024168662, -2.080538600569502794, -5.783357778048658027 ) ) ;
#2369 = CARTESIAN_POINT ( 'NONE',  ( 32.97211790677835097, -2.610546234160043610, -8.283357778048658915 ) ) ;
#2370 = CARTESIAN_POINT ( 'NONE',  ( 27.55969062878875064, -7.234529412811931515, -5.783357778048668685 ) ) ;
#2371 = CARTESIAN_POINT ( 'NONE',  ( 0.000000000000000000, 0.000000000000000000, -3.000000000000002665 ) ) ;
#2372 = AXIS2_PLACEMENT_3D ( 'NONE', #8904, #6081, #2207 ) ;
#2373 = CARTESIAN_POINT ( 'NONE',  ( -15.38839387855823126, 12.77214111725050216, 16.22946975555079163 ) ) ;
#2374 = SURFACE_STYLE_USAGE ( .BOTH. , #14785 ) ;
#2375 = CARTESIAN_POINT ( 'NONE',  ( 31.66930131758986988, -2.967382423816733894, -3.627061608673662008 ) ) ;
#2376 = CARTESIAN_POINT ( 'NONE',  ( 31.65190802758064592, -5.477360103042387074, -7.939653947423662927 ) ) ;
#2377 = ORIENTED_EDGE ( 'NONE', *, *, #5084, .T. ) ;
#2378 = AXIS2_PLACEMENT_3D ( 'NONE', #12332, #17897, #10945 ) ;
#2379 = CARTESIAN_POINT ( 'NONE',  ( 26.82912971812490355, -6.258282166232842947, 3.283357778048663800 ) ) ;
#2380 =( BOUNDED_CURVE ( )  B_SPLINE_CURVE ( 2, ( #5842, #13828, #11000, #1691, #5747, #15374, #237, #1415, #11260 ),
 .UNSPECIFIED., .F., .T. ) 
 B_SPLINE_CURVE_WITH_KNOTS ( ( 3, 2, 2, 2, 3 ),
 ( 0.2115384615384615641, 0.2179487179487179516, 0.2307692307692307820, 0.2435897435897435848, 0.2500000000000000000 ),
 .UNSPECIFIED. ) 
 CURVE ( )  GEOMETRIC_REPRESENTATION_ITEM ( )  RATIONAL_B_SPLINE_CURVE ( ( 0.9330127018922194093, 0.9330127018922196314, 1.000000000000000000, 0.8660254037844387076, 1.000000000000000000, 0.8660254037844387076, 1.000000000000000000, 0.9330127018922191873, 0.9330127018922194093 ) ) 
 REPRESENTATION_ITEM ( '' )  );
#2381 = ORIENTED_EDGE ( 'NONE', *, *, #14225, .F. ) ;
#2382 = EDGE_CURVE ( 'NONE', #11016, #11836, #4106, .T. ) ;
#2383 = CARTESIAN_POINT ( 'NONE',  ( 26.03726795043090547, -3.446058701420613879, 3.283357778048666464 ) ) ;
#2384 = MECHANICAL_DESIGN_GEOMETRIC_PRESENTATION_REPRESENTATION (  '', ( #3231 ), #5206 ) ;
#2385 = CARTESIAN_POINT ( 'NONE',  ( 29.60297508593253468, -5.724216059278466773, -7.939653947423662927 ) ) ;
#2386 = CARTESIAN_POINT ( 'NONE',  ( 27.90727577511918867, -2.156494279411373061, 5.783357778048657138 ) ) ;
#2387 = DIRECTION ( 'NONE',  ( -0.5000000000000051070, 0.000000000000000000, 0.8660254037844355990 ) ) ;
#2388 = CARTESIAN_POINT ( 'NONE',  ( 27.99987602667382802, -2.482696394238434578, -4.533357778048659803 ) ) ;
#2389 = AXIS2_PLACEMENT_3D ( 'NONE', #16083, #3561, #10523 ) ;
#2390 = CARTESIAN_POINT ( 'NONE',  ( 3.522881874163251492, -2.820349071480749537, -3.298443181295994009 ) ) ;
#2391 = CARTESIAN_POINT ( 'NONE',  ( 30.49166216014303643, -4.363205751385915931, -8.283357778048662468 ) ) ;
#2392 = CARTESIAN_POINT ( 'NONE',  ( 32.97402322492378346, -4.064130265842336165, -3.627061608673664672 ) ) ;
#2393 = AXIS2_PLACEMENT_3D ( 'NONE', #12034, #14690, #17622 ) ;
#2394 = LINE ( 'NONE', #1024, #338 ) ;
#2395 = CARTESIAN_POINT ( 'NONE',  ( 32.60321786976872005, -6.626883982076972934, -5.783357778048663356 ) ) ;
#2396 = CARTESIAN_POINT ( 'NONE',  ( 27.17934203385504333, -30.00000000000000355, -13.93658524716016878 ) ) ;
#2397 = PLANE ( 'NONE',  #15592 ) ;
#2398 = CARTESIAN_POINT ( 'NONE',  ( 33.30246708102489350, -5.905470865888903020, -4.705209693361168455 ) ) ;
#2399 = AXIS2_PLACEMENT_3D ( 'NONE', #2434, #10734, #2509 ) ;
#2400 = VECTOR ( 'NONE', #12040, 1000.000000000000000 ) ;
#2401 = ADVANCED_FACE ( 'NONE', ( #16331 ), #14949, .T. ) ;
#2402 = CARTESIAN_POINT ( 'NONE',  ( 30.52163964716380917, -2.178873678870954400, 7.033357778048666020 ) ) ;
#2403 = VERTEX_POINT ( 'NONE', #13592 ) ;
#2404 = DIRECTION ( 'NONE',  ( 1.000000000000000000, 0.000000000000000000, 0.000000000000000000 ) ) ;
#2405 = DIRECTION ( 'NONE',  ( 0.000000000000000000, 0.000000000000000000, 1.000000000000000000 ) ) ;
#2406 = CARTESIAN_POINT ( 'NONE',  ( 33.13163345120441505, -4.045141346131868154, -3.627061608673664672 ) ) ;
#2407 = PLANE ( 'NONE',  #4145 ) ;
#2408 = EDGE_CURVE ( 'NONE', #16712, #14075, #6866, .T. ) ;
#2409 = CARTESIAN_POINT ( 'NONE',  ( 25.61697401368257587, -3.496695820648536568, -3.283357778048662023 ) ) ;
#2410 = DIRECTION ( 'NONE',  ( -1.000000000000000000, 0.000000000000000000, 0.000000000000000000 ) ) ;
#2411 = CARTESIAN_POINT ( 'NONE',  ( -11.29999999999999893, 0.000000000000000000, 0.000000000000000000 ) ) ;
#2412 = CARTESIAN_POINT ( 'NONE',  ( 26.18940075748478691, -6.337263906362392341, -7.823530922983556124 ) ) ;
#2413 = CARTESIAN_POINT ( 'NONE',  ( 29.34898802046944155, -4.500875419183088866, -3.627061608673664672 ) ) ;
#2414 = CARTESIAN_POINT ( 'NONE',  ( 31.03206908560819954, -5.751910973953720863, 8.283357778048658915 ) ) ;
#2415 = ORIENTED_EDGE ( 'NONE', *, *, #10044, .T. ) ;
#2416 = ORIENTED_EDGE ( 'NONE', *, *, #6251, .T. ) ;
#2417 = ADVANCED_FACE ( 'NONE', ( #17882 ), #1174, .T. ) ;
#2418 = CARTESIAN_POINT ( 'NONE',  ( 29.15206445563513071, -6.405512418264540209, 4.705209693361159573 ) ) ;
#2419 = DIRECTION ( 'NONE',  ( 0.000000000000000000, 0.000000000000000000, -1.000000000000000000 ) ) ;
#2420 = DIRECTION ( 'NONE',  ( -1.000000000000000000, 0.000000000000000000, 0.000000000000000000 ) ) ;
#2421 = ORIENTED_EDGE ( 'NONE', *, *, #3769, .F. ) ;
#2422 = CARTESIAN_POINT ( 'NONE',  ( 33.15485366002904755, -6.560422763297783177, -5.783357778048663356 ) ) ;
#2423 = LINE ( 'NONE', #14669, #867 ) ;
#2425 = AXIS2_PLACEMENT_3D ( 'NONE', #3894, #12492, #17884 ) ;
#2424 = FACE_OUTER_BOUND ( 'NONE', #2744, .T. ) ;
#2426 = CARTESIAN_POINT ( 'NONE',  ( 31.69574812466957781, -6.726019302751734763, -5.783357778048669573 ) ) ;
#2427 = ADVANCED_FACE ( 'NONE', ( #16579 ), #12226, .T. ) ;
#2428 = ORIENTED_EDGE ( 'NONE', *, *, #12252, .T. ) ;
#2429 = CARTESIAN_POINT ( 'NONE',  ( 31.32102116884452414, -5.717097954277069682, 3.283357778048663356 ) ) ;
#2430 = PLANE ( 'NONE',  #8384 ) ;
#2431 = SURFACE_STYLE_FILL_AREA ( #17320 ) ;
#2432 = CARTESIAN_POINT ( 'NONE',  ( 26.84461768998868436, -2.294720455324902542, 5.783357778048668685 ) ) ;
#2433 = ORIENTED_EDGE ( 'NONE', *, *, #10552, .F. ) ;
#2434 = CARTESIAN_POINT ( 'NONE',  ( -20.00000000000000000, -30.00000000000000355, -17.00000000000000000 ) ) ;
#2435 = CARTESIAN_POINT ( 'NONE',  ( 31.34233605952372415, -6.778795339760710803, -5.783357778048663356 ) ) ;
#2436 = CARTESIAN_POINT ( 'NONE',  ( 33.06225340847440464, -6.234220648470727433, -4.533357778048668685 ) ) ;
#2437 = CARTESIAN_POINT ( 'NONE',  ( 27.57216386142120257, -6.895668018177890879, 4.533357778048659803 ) ) ;
#2438 = VERTEX_POINT ( 'NONE', #16490 ) ;
#2439 = EDGE_LOOP ( 'NONE', ( #16960, #1721, #17284, #3294 ) ) ;
#2440 = ADVANCED_FACE ( 'NONE', ( #9573 ), #15125, .F. ) ;
#2441 = EDGE_LOOP ( 'NONE', ( #11394, #4885, #245, #3297 ) ) ;
#2442 = CARTESIAN_POINT ( 'NONE',  ( 31.39792096211754924, -4.254019462947003838, 3.627061608673664228 ) ) ;
#2443 = CARTESIAN_POINT ( 'NONE',  ( 30.40841950734487753, -3.119293781500474427, 7.939653947423662927 ) ) ;
#2444 = ORIENTED_EDGE ( 'NONE', *, *, #992, .F. ) ;
#2445 = CARTESIAN_POINT ( 'NONE',  ( 31.26353094466156080, -6.788289799823394866, -5.783357778048663356 ) ) ;
#2446 = CARTESIAN_POINT ( 'NONE',  ( 29.78612525785423060, -2.267488637519798012, -7.033357778048658027 ) ) ;
#2447 = DIRECTION ( 'NONE',  ( -0.1196152422706610735, 0.9928203230275511881, 0.000000000000000000 ) ) ;
#2448 = CARTESIAN_POINT ( 'NONE',  ( 28.28955653359400557, -5.882457056865704637, -3.627061608673668225 ) ) ;
#2449 = DIRECTION ( 'NONE',  ( -1.000000000000000000, -0.000000000000000000, -0.000000000000000000 ) ) ;
#2450 = ADVANCED_FACE ( 'NONE', ( #5496 ), #13939, .F. ) ;
#2451 = CARTESIAN_POINT ( 'NONE',  ( 33.14105852333657509, -6.224726188408045147, -4.533357778048668685 ) ) ;
#2452 = CARTESIAN_POINT ( 'NONE',  ( 31.66176685062031027, -1.704152250161192539, 5.113484796970859669 ) ) ;
#2453 = CARTESIAN_POINT ( 'NONE',  ( 19.22414633752738666, -11.22056979495215145, 15.64782563911137814 ) ) ;
#2454 =( NAMED_UNIT ( * ) PLANE_ANGLE_UNIT ( ) SI_UNIT ( $, .RADIAN. ) );
#2455 = ORIENTED_EDGE ( 'NONE', *, *, #12047, .T. ) ;
#2456 = EDGE_CURVE ( 'NONE', #6239, #17548, #9643, .T. ) ;
#2457 = CARTESIAN_POINT ( 'NONE',  ( 30.41294626588012306, -6.253601060580800564, -6.861505862736167138 ) ) ;
#2458 = CARTESIAN_POINT ( 'NONE',  ( 33.54323074294813267, -5.249493066516778050, -7.939653947423662927 ) ) ;
#2459 = ORIENTED_EDGE ( 'NONE', *, *, #6673, .F. ) ;
#2460 = CARTESIAN_POINT ( 'NONE',  ( 31.74131510559286085, -5.666460835049167422, 8.283357778048660691 ) ) ;
#2461 = CARTESIAN_POINT ( 'NONE',  ( 25.71748644841968456, -2.420320648352046078, 5.783357778048663356 ) ) ;
#2462 = EDGE_CURVE ( 'NONE', #14411, #17313, #11338, .T. ) ;
#2463 = ORIENTED_EDGE ( 'NONE', *, *, #10233, .T. ) ;
#2464 = CARTESIAN_POINT ( 'NONE',  ( 30.67110321781257909, -3.087645581983020637, 3.627061608673666449 ) ) ;
#2465 = CARTESIAN_POINT ( 'NONE',  ( 28.13194630731337753, -5.901445976576172647, -3.627061608673667781 ) ) ;
#2466 = DIRECTION ( 'NONE',  ( 1.000000000000000000, 0.000000000000000000, 0.000000000000000000 ) ) ;
#2467 = CARTESIAN_POINT ( 'NONE',  ( 26.01595305975170547, -2.384361315936983416, -5.783357778048670461 ) ) ;
#2468 = CARTESIAN_POINT ( 'NONE',  ( 27.93543013035303701, -2.153102235610331316, -5.113484796970857893 ) ) ;
#2469 = CARTESIAN_POINT ( 'NONE',  ( 2.500000000000000000, -1.178949249685218081, -2.041999999999998039 ) ) ;
#2470 = CARTESIAN_POINT ( 'NONE',  ( 32.89331279191618762, -2.620040694222726785, -8.283357778048658915 ) ) ;
#2471 = EDGE_CURVE ( 'NONE', #1158, #1034, #7607, .T. ) ;
#2472 = CARTESIAN_POINT ( 'NONE',  ( 32.64557936882268052, -2.222789665795767089, -4.705209693361161349 ) ) ;
#2473 = CARTESIAN_POINT ( 'NONE',  ( -35.74085044863416272, -23.57886868891566223, -11.27079897466147607 ) ) ;
#2474 = CARTESIAN_POINT ( 'NONE',  ( 30.66124439477291475, -6.860853434864224276, -6.453230759126470595 ) ) ;
#2475 = FACE_OUTER_BOUND ( 'NONE', #9632, .T. ) ;
#2476 = CARTESIAN_POINT ( 'NONE',  ( 26.30185955129047315, -7.986322017489088765, -6.648778972250404706 ) ) ;
#2477 = CARTESIAN_POINT ( 'NONE',  ( 32.67202617590239555, -5.981426544730773287, -4.705209693361168455 ) ) ;
#2478 = EDGE_CURVE ( 'NONE', #6885, #5290, #17097, .T. ) ;
#2479 = CARTESIAN_POINT ( 'NONE',  ( 32.30788887834420819, -1.963665922152317833, -7.033357778048658027 ) ) ;
#2480 = DIRECTION ( 'NONE',  ( -1.000000000000000000, 0.000000000000000000, 0.000000000000000000 ) ) ;
#2481 = ORIENTED_EDGE ( 'NONE', *, *, #11895, .F. ) ;
#2482 = CARTESIAN_POINT ( 'NONE',  ( 0.000000000000000000, 0.000000000000000000, -10.00000000000000000 ) ) ;
#2483 = DIRECTION ( 'NONE',  ( -0.7071067811865489050, 8.659560562354950115E-17, 0.7071067811865462405 ) ) ;
#2484 = DIRECTION ( 'NONE',  ( 1.000000000000000000, 0.000000000000000000, 0.000000000000000000 ) ) ;
#2485 = EDGE_CURVE ( 'NONE', #987, #4619, #6458, .T. ) ;
#2486 = CARTESIAN_POINT ( 'NONE',  ( 26.83664947211162399, -6.984282976826746037, -4.533357778048668685 ) ) ;
#2487 = CARTESIAN_POINT ( 'NONE',  ( 30.63309003953906995, -6.864245478665264244, 5.783357778048664244 ) ) ;
#2488 = CARTESIAN_POINT ( 'NONE',  ( 0.2500000000000002220, 0.000000000000000000, 0.000000000000000000 ) ) ;
#2489 = CARTESIAN_POINT ( 'NONE',  ( 33.48996557372703364, -1.821249024531260696, -7.033357778048658027 ) ) ;
#2490 = CARTESIAN_POINT ( 'NONE',  ( 27.95193767517966776, -20.05341752217977103, -13.73231903009881627 ) ) ;
#2491 = CARTESIAN_POINT ( 'NONE',  ( 32.57067411085063924, -7.020353038355215070, 5.783357778048657138 ) ) ;
#2492 = ORIENTED_EDGE ( 'NONE', *, *, #265, .T. ) ;
#2493 = CARTESIAN_POINT ( 'NONE',  ( 29.34898802046944155, -4.500875419183088866, 7.939653947423662039 ) ) ;
#2494 = SURFACE_STYLE_FILL_AREA ( #4027 ) ;
#2495 = CARTESIAN_POINT ( 'NONE',  ( 21.42986351335030548, -22.27113001973728146, 15.24426822127429659 ) ) ;
#2496 = VERTEX_POINT ( 'NONE', #6178 ) ;
#2497 = DIRECTION ( 'NONE',  ( -0.000000000000000000, -0.000000000000000000, 1.000000000000000000 ) ) ;
#2498 = ORIENTED_EDGE ( 'NONE', *, *, #11162, .T. ) ;
#2499 = CARTESIAN_POINT ( 'NONE',  ( 27.87986455999572399, -6.131689368163070419, -3.283357778048667797 ) ) ;
#2500 = VERTEX_POINT ( 'NONE', #3463 ) ;
#2501 = DIRECTION ( 'NONE',  ( -1.000000000000000000, 0.000000000000000000, 0.000000000000000000 ) ) ;
#2502 = CARTESIAN_POINT ( 'NONE',  ( 29.55043834383899437, -5.730545699181964991, -3.627061608673668225 ) ) ;
#2503 = LINE ( 'NONE', #8213, #15307 ) ;
#2504 = DIRECTION ( 'NONE',  ( -0.000000000000000000, -0.000000000000000000, -1.000000000000000000 ) ) ;
#2505 = CARTESIAN_POINT ( 'NONE',  ( 33.14105852333657509, -6.224726188408045147, 7.033357778048657138 ) ) ;
#2506 = ORIENTED_EDGE ( 'NONE', *, *, #17430, .T. ) ;
#2507 = CARTESIAN_POINT ( 'NONE',  ( 30.25533603959949502, -6.272589980291270351, 4.705209693361160461 ) ) ;
#2508 = EDGE_CURVE ( 'NONE', #9311, #17066, #4894, .T. ) ;
#2509 = DIRECTION ( 'NONE',  ( 0.9396926207859104263, 0.000000000000000000, -0.3420201433256631063 ) ) ;
#2510 = CARTESIAN_POINT ( 'NONE',  ( 30.88568772756644520, -4.315733451902305617, -3.283357778048664688 ) ) ;
#2511 = DIRECTION ( 'NONE',  ( 0.000000000000000000, 0.5000000000000011102, 0.8660254037844380415 ) ) ;
#2512 = CARTESIAN_POINT ( 'NONE',  ( 29.18947247604337392, -3.066280307211263878, 3.283357778048666464 ) ) ;
#2513 = VERTEX_POINT ( 'NONE', #4808 ) ;
#2514 = EDGE_CURVE ( 'NONE', #4496, #15456, #3727, .T. ) ;
#2515 = EDGE_LOOP ( 'NONE', ( #5955, #482 ) ) ;
#2516 = ORIENTED_EDGE ( 'NONE', *, *, #14445, .F. ) ;
#2517 = CARTESIAN_POINT ( 'NONE',  ( 32.77709966008947617, -5.968767264923789284, 4.705209693361160461 ) ) ;
#2518 = CARTESIAN_POINT ( 'NONE',  ( -2.749999999999992895, -20.49999999999999645, -6.000000000000000000 ) ) ;
#2519 = CARTESIAN_POINT ( 'NONE',  ( 31.04338717100262102, -6.177645381738930297, 4.705209693361159573 ) ) ;
#2520 = ORIENTED_EDGE ( 'NONE', *, *, #1638, .F. ) ;
#2521 = DIRECTION ( 'NONE',  ( 0.9928203230275511881, 0.1196152422706610735, 9.614813431917827710E-17 ) ) ;
#2522 = CARTESIAN_POINT ( 'NONE',  ( 27.53837573810955419, -6.172832027328289506, -8.283357778048664244 ) ) ;
#2523 = CARTESIAN_POINT ( 'NONE',  ( 28.39010325924584421, -2.735490497978389612, -4.705209693361160461 ) ) ;
#2524 = CARTESIAN_POINT ( 'NONE',  ( 28.67914455963771303, -4.581578327848842669, -8.283357778048662468 ) ) ;
#2525 = CARTESIAN_POINT ( 'NONE',  ( 32.14656953781143756, -4.163822094218565972, -3.283357778048664688 ) ) ;
#2526 = CARTESIAN_POINT ( 'NONE',  ( 26.01652455409633902, -4.902371455920926380, -5.783357778048663356 ) ) ;
#2527 = VECTOR ( 'NONE', #3474, 1000.000000000000000 ) ;
#2528 = CARTESIAN_POINT ( 'NONE',  ( 1.747541505913277948, -3.837784562140266864, -3.203702292528911144 ) ) ;
#2529 = LINE ( 'NONE', #15127, #394 ) ;
#2530 = PRESENTATION_STYLE_ASSIGNMENT (( #15260 ) ) ;
#2531 = EDGE_CURVE ( 'NONE', #5172, #3447, #14651, .T. ) ;
#2532 = CARTESIAN_POINT ( 'NONE',  ( 32.95662993491455950, -6.574107945067995118, -5.783357778048669573 ) ) ;
#2533 = CARTESIAN_POINT ( 'NONE',  ( 28.26310972651430120, -2.123820177930694442, -5.783357778048658915 ) ) ;
#2534 = EDGE_CURVE ( 'NONE', #9939, #10468, #10447, .T. ) ;
#2535 = CARTESIAN_POINT ( 'NONE',  ( 35.74085044863416982, -23.57886868891565513, -11.27079897466147251 ) ) ;
#2536 = CARTESIAN_POINT ( 'NONE',  ( -3.000000000000000000, 3.673940397442059868E-16, 2.399999999999999467 ) ) ;
#2537 = B_SPLINE_CURVE_WITH_KNOTS ( 'NONE', 3,
 ( #10607, #3656, #9261, #14806, #16264, #3836, #1106, #2557 ),
 .UNSPECIFIED., .F., .F.,
 ( 4, 2, 2, 4 ),
 ( 2.465131517092369892E-07, 0.001183067374689850647, 0.001774477805458921347, 0.002365888236227992047 ),
 .UNSPECIFIED. ) ;
#2538 = EDGE_CURVE ( 'NONE', #9123, #16897, #3649, .T. ) ;
#2539 = EDGE_CURVE ( 'NONE', #6798, #6479, #11500, .T. ) ;
#2540 = ORIENTED_EDGE ( 'NONE', *, *, #5351, .F. ) ;
#2541 = AXIS2_PLACEMENT_3D ( 'NONE', #14177, #10351, #17285 ) ;
#2542 = VERTEX_POINT ( 'NONE', #6277 ) ;
#2543 = CARTESIAN_POINT ( 'NONE',  ( 30.78070346053490880, -6.209293581256383199, 6.861505862736158257 ) ) ;
#2544 = CARTESIAN_POINT ( 'NONE',  ( 28.87615734162756453, -4.557842178314484016, -7.939653947423662039 ) ) ;
#2545 = CARTESIAN_POINT ( 'NONE',  ( 27.65467808709180630, -4.705006306174339237, 8.283357778048662468 ) ) ;
#2546 = CARTESIAN_POINT ( 'NONE',  ( 8.776279441628796363, -6.799038105676699750, -3.000000000000000888 ) ) ;
#2547 = FACE_OUTER_BOUND ( 'NONE', #16682, .T. ) ;
#2548 = CARTESIAN_POINT ( 'NONE',  ( 25.75668387115780078, -2.745663783273349701, 5.876686579351208195 ) ) ;
#2549 = DIRECTION ( 'NONE',  ( -0.000000000000000000, 1.000000000000000000, 0.000000000000000000 ) ) ;
#2550 = CARTESIAN_POINT ( 'NONE',  ( 31.59864285835955400, -2.049116061056871274, -7.033357778048658027 ) ) ;
#2551 = ORIENTED_EDGE ( 'NONE', *, *, #6329, .T. ) ;
#2552 = CIRCLE ( 'NONE', #6612, 2.700000000000000622 ) ;
#2553 = VERTEX_POINT ( 'NONE', #13174 ) ;
#2554 = ORIENTED_EDGE ( 'NONE', *, *, #13467, .F. ) ;
#2555 = CARTESIAN_POINT ( 'NONE',  ( 32.12473870642251939, -5.420393343910986594, -7.939653947423664704 ) ) ;
#2556 = CARTESIAN_POINT ( 'NONE',  ( 0.000000000000000000, 0.000000000000000000, 0.000000000000000000 ) ) ;
#2557 = CARTESIAN_POINT ( 'NONE',  ( 2.000000000000006217, 3.464101615137751722, -1.401678602859870442E-15 ) ) ;
#2558 = DIRECTION ( 'NONE',  ( 1.000000000000000000, 7.105427357601001859E-15, 0.000000000000000000 ) ) ;
#2559 = FACE_OUTER_BOUND ( 'NONE', #6639, .T. ) ;
#2560 = CARTESIAN_POINT ( 'NONE',  ( 33.40301380667672504, -2.758504307001591993, -3.627061608673662896 ) ) ;
#2561 = VECTOR ( 'NONE', #287, 1000.000000000000114 ) ;
#2562 = CARTESIAN_POINT ( 'NONE',  ( 32.61569110240115776, -6.288022587442930522, -7.033357778048666908 ) ) ;
#2563 = CIRCLE ( 'NONE', #9223, 5.000000000000000000 ) ;
#2564 = ADVANCED_FACE ( 'NONE', ( #3737 ), #2962, .T. ) ;
#2565 = CARTESIAN_POINT ( 'NONE',  ( -45.00000000000000711, -16.03270077640482683, 0.5379818257722508434 ) ) ;
#2566 = AXIS2_PLACEMENT_3D ( 'NONE', #17401, #3402, #11731 ) ;
#2567 = ORIENTED_EDGE ( 'NONE', *, *, #17594, .F. ) ;
#2568 = CARTESIAN_POINT ( 'NONE',  ( 25.83183225892937784, -3.369404079293177201, 4.123432853728487224 ) ) ;
#2569 = CARTESIAN_POINT ( 'NONE',  ( 29.34898802046944155, -4.500875419183088866, -3.627061608673664672 ) ) ;
#2570 = DIRECTION ( 'NONE',  ( 0.000000000000000000, -1.000000000000000000, 1.287488025362403787E-15 ) ) ;
#2571 = EDGE_LOOP ( 'NONE', ( #10653, #1537, #14301, #6626 ) ) ;
#2572 = CARTESIAN_POINT ( 'NONE',  ( 26.97551107961034944, -7.694459687869362519, -5.783357778048669573 ) ) ;
#2573 = CARTESIAN_POINT ( 'NONE',  ( 3.248936832696173393, -30.00000000000000355, -78.00000000000000000 ) ) ;
#2574 = LINE ( 'NONE', #8461, #13241 ) ;
#2575 = CARTESIAN_POINT ( 'NONE',  ( 33.76397967447234549, -5.422769698972272678, -8.283357778048662468 ) ) ;
#2576 = AXIS2_PLACEMENT_3D ( 'NONE', #15181, #3944, #2420 ) ;
#2577 = CARTESIAN_POINT ( 'NONE',  ( 34.25812524399339765, -6.427500325324518649, 5.783357778048663356 ) ) ;
#2578 = CARTESIAN_POINT ( 'NONE',  ( 31.80137159822941939, -6.386132006154467078, 7.033357778048657138 ) ) ;
#2579 = ORIENTED_EDGE ( 'NONE', *, *, #7647, .T. ) ;
#2580 = ADVANCED_FACE ( 'NONE', ( #2475 ), #5171, .F. ) ;
#2581 = CARTESIAN_POINT ( 'NONE',  ( 30.80679339554874119, -2.444327062417882779, 4.705209693361168455 ) ) ;
#2582 = CARTESIAN_POINT ( 'NONE',  ( -16.75000000000000000, -16.21813761408365195, 16.03574476417183448 ) ) ;
#2583 = CARTESIAN_POINT ( 'NONE',  ( 21.62682814333776804, -22.31876753225984800, 15.20565444446567227 ) ) ;
#2584 = EDGE_CURVE ( 'NONE', #3798, #6225, #14837, .T. ) ;
#2585 = ORIENTED_EDGE ( 'NONE', *, *, #15391, .F. ) ;
#2586 = ORIENTED_EDGE ( 'NONE', *, *, #9191, .T. ) ;
#2587 = AXIS2_PLACEMENT_3D ( 'NONE', #7356, #12872, #11487 ) ;
#2588 = CARTESIAN_POINT ( 'NONE',  ( 34.25812524399339765, -6.427500325324518649, -5.783357778048663356 ) ) ;
#2589 = EDGE_LOOP ( 'NONE', ( #534, #1950, #17877 ) ) ;
#2590 = DIRECTION ( 'NONE',  ( -0.000000000000000000, -0.000000000000000000, -1.000000000000000000 ) ) ;
#2591 = CARTESIAN_POINT ( 'NONE',  ( 29.66420847303068697, -4.462897579762144851, -7.939653947423662039 ) ) ;
#2592 = CARTESIAN_POINT ( 'NONE',  ( -8.632250723006720250, -18.84644399697197770, -13.00000000000000178 ) ) ;
#2593 = DIRECTION ( 'NONE',  ( -0.9928203230275510771, -0.1196152422706614760, -0.000000000000000000 ) ) ;
#2594 = DIRECTION ( 'NONE',  ( 0.000000000000000000, 0.000000000000000000, 1.000000000000000000 ) ) ;
#2595 = DIRECTION ( 'NONE',  ( 0.000000000000000000, 1.000000000000000000, 0.000000000000000000 ) ) ;
#2596 = PRODUCT_DEFINITION_SHAPE ( 'NONE', 'NONE',  #17981 ) ;
#2597 = CARTESIAN_POINT ( 'NONE',  ( 28.77978050244509944, -3.315512618508630993, 3.627061608673666893 ) ) ;
#2598 = DIRECTION ( 'NONE',  ( 0.9237280213470682178, 0.3830490080632377170, 0.000000000000000000 ) ) ;
#2599 = DIRECTION ( 'NONE',  ( -0.1196152422706610735, 0.9928203230275511881, 0.000000000000000000 ) ) ;
#2600 = CARTESIAN_POINT ( 'NONE',  ( 38.42250453410443356, 0.8083635290851024502, -5.533357778048658027 ) ) ;
#2601 = ORIENTED_EDGE ( 'NONE', *, *, #7106, .T. ) ;
#2602 = CARTESIAN_POINT ( 'NONE',  ( 30.09392748191118017, -6.591845302810410701, 4.533357778048659803 ) ) ;
#2603 = AXIS2_PLACEMENT_3D ( 'NONE', #10559, #13479, #14591 ) ;
#2604 = ORIENTED_EDGE ( 'NONE', *, *, #15533, .F. ) ;
#2605 = ORIENTED_EDGE ( 'NONE', *, *, #6651, .F. ) ;
#2606 = ORIENTED_EDGE ( 'NONE', *, *, #13713, .F. ) ;
#2607 = EDGE_CURVE ( 'NONE', #15344, #11718, #10187, .T. ) ;
#2608 = CARTESIAN_POINT ( 'NONE',  ( 32.67202617590239555, -5.981426544730773287, 6.861505862736158257 ) ) ;
#2609 = CARTESIAN_POINT ( 'NONE',  ( 27.10304229683147526, -4.771467524953526329, 8.283357778048662468 ) ) ;
#2610 = ORIENTED_EDGE ( 'NONE', *, *, #4394, .F. ) ;
#2611 = AXIS2_PLACEMENT_3D ( 'NONE', #5101, #13275, #11907 ) ;
#2612 = CARTESIAN_POINT ( 'NONE',  ( 30.28142597461332741, -2.507623461452779701, 6.861505862736166250 ) ) ;
#2613 = DIRECTION ( 'NONE',  ( -0.3830490080632376615, 0.9237280213470682178, 0.000000000000000000 ) ) ;
#2614 = CARTESIAN_POINT ( 'NONE',  ( 0.000000000000000000, 0.000000000000000000, -9.600000000000001421 ) ) ;
#2615 = DIRECTION ( 'NONE',  ( 1.000000000000000000, 0.000000000000000000, 0.000000000000000000 ) ) ;
#2616 = CARTESIAN_POINT ( 'NONE',  ( 26.60838078660069428, -6.085005533777348319, -7.939653947423664704 ) ) ;
#2617 = CARTESIAN_POINT ( 'NONE',  ( 28.83304567166618781, -6.743756660494150346, -7.033357778048666908 ) ) ;
#2618 = CARTESIAN_POINT ( 'NONE',  ( 29.21955148510287614, -5.970283550416647600, -3.283357778048667797 ) ) ;
#2619 = FACE_OUTER_BOUND ( 'NONE', #582, .T. ) ;
#2620 = B_SPLINE_CURVE_WITH_KNOTS ( 'NONE', 3,
 ( #11816, #17395, #9022, #10275, #3667, #14650, #12000, #768 ),
 .UNSPECIFIED., .F., .F.,
 ( 4, 2, 2, 4 ),
 ( 0.000000000000000000, 0.002450665683189819262, 0.003675998524784728893, 0.004901331366379638524 ),
 .UNSPECIFIED. ) ;
#2621 = CARTESIAN_POINT ( 'NONE',  ( 19.22414633752738666, -11.22056979495215145, -15.64782563911137814 ) ) ;
#2622 = CYLINDRICAL_SURFACE ( 'NONE', #2134, 2.500000000000001776 ) ;
#2623 = ADVANCED_FACE ( 'NONE', ( #12156 ), #5002, .T. ) ;
#2624 =( NAMED_UNIT ( * ) SI_UNIT ( $, .STERADIAN. ) SOLID_ANGLE_UNIT ( ) );
#2625 = EDGE_LOOP ( 'NONE', ( #3898, #4989 ) ) ;
#2626 = CARTESIAN_POINT ( 'NONE',  ( 29.97942892559193950, -4.424919740341219487, -3.627061608673664672 ) ) ;
#2627 = STYLED_ITEM ( 'NONE', ( #17931 ), #11433 ) ;
#2628 = CARTESIAN_POINT ( 'NONE',  ( 27.63266882139180325, -2.199775856772564708, -5.783357778048658915 ) ) ;
#2629 = VECTOR ( 'NONE', #10486, 1000.000000000000227 ) ;
#2630 = CARTESIAN_POINT ( 'NONE',  ( 33.95908713831673964, -3.945449517755637014, -5.783357778048663356 ) ) ;
#2631 = PLANE ( 'NONE',  #8134 ) ;
#2632 = AXIS2_PLACEMENT_3D ( 'NONE', #112, #391, #5897 ) ;
#2633 = VERTEX_POINT ( 'NONE', #2396 ) ;
#2634 = CARTESIAN_POINT ( 'NONE',  ( 25.71748644841968456, -2.420320648352046078, 5.783357778048663356 ) ) ;
#2635 = CARTESIAN_POINT ( 'NONE',  ( 26.98483462626008134, -4.785709214840094816, -7.939653947423662039 ) ) ;
#2636 = EDGE_CURVE ( 'NONE', #7694, #1336, #12263, .T. ) ;
#2637 = CARTESIAN_POINT ( 'NONE',  ( 8.874038404635971489, 3.391377654146752629, -2.000000000000000000 ) ) ;
#2638 = LINE ( 'NONE', #12053, #5235 ) ;
#2639 = CARTESIAN_POINT ( 'NONE',  ( 28.13194630731337753, -5.901445976576171759, -3.627061608673667781 ) ) ;
#2640 = DIRECTION ( 'NONE',  ( 0.9928203230275510771, 0.1196152422706609902, 4.006172263299092517E-17 ) ) ;
#2641 = CARTESIAN_POINT ( 'NONE',  ( 9.500000000000000000, 1.163414459189985485E-15, 0.000000000000000000 ) ) ;
#2642 = CONICAL_SURFACE ( 'NONE', #7278, 3.999999999999998224, 0.8911886515913775009 ) ;
#2643 = FACE_BOUND ( 'NONE', #2625, .T. ) ;
#2644 = CARTESIAN_POINT ( 'NONE',  ( 29.04309111455793513, -1.630102785574754742, -5.783357778048658027 ) ) ;
#2645 = EDGE_CURVE ( 'NONE', #9826, #1069, #3570, .T. ) ;
#2646 = EDGE_LOOP ( 'NONE', ( #1255, #9227, #4565, #15437 ) ) ;
#2647 = DIRECTION ( 'NONE',  ( -1.000000000000000000, 0.000000000000000000, 0.000000000000000000 ) ) ;
#2648 = DIRECTION ( 'NONE',  ( -1.000000000000000000, 0.000000000000000000, 0.000000000000000000 ) ) ;
#2649 = DIRECTION ( 'NONE',  ( -0.1196152422706610735, 0.9928203230275511881, 0.000000000000000000 ) ) ;
#2650 = LINE ( 'NONE', #12157, #17653 ) ;
#2651 = SHAPE_REPRESENTATION ( 'Bleed Screw Nipple', ( #3575 ), #12173 ) ;
#2652 = CARTESIAN_POINT ( 'NONE',  ( 29.50659824675005893, -4.481886499472614638, -7.939653947423662039 ) ) ;
#2653 = AXIS2_PLACEMENT_3D ( 'NONE', #11618, #6546, #17738 ) ;
#2654 = DIRECTION ( 'NONE',  ( 0.000000000000000000, 1.000000000000000000, 0.000000000000000000 ) ) ;
#2655 = VECTOR ( 'NONE', #4703, 1000.000000000000000 ) ;
#2656 = EDGE_CURVE ( 'NONE', #757, #9716, #17174, .T. ) ;
#2657 = VERTEX_POINT ( 'NONE', #6548 ) ;
#2658 = CARTESIAN_POINT ( 'NONE',  ( 5.237433445017501299, -16.51494876461869410, -16.99438405180048761 ) ) ;
#2659 = ORIENTED_EDGE ( 'NONE', *, *, #10282, .T. ) ;
#2660 =( NAMED_UNIT ( * ) SI_UNIT ( $, .STERADIAN. ) SOLID_ANGLE_UNIT ( ) );
#2661 = CARTESIAN_POINT ( 'NONE',  ( 30.30787278169304244, -6.266260340387784566, -4.705209693361169343 ) ) ;
#2662 = CARTESIAN_POINT ( 'NONE',  ( 26.01652455409633902, -4.902371455920928156, -5.783357778048663356 ) ) ;
#2663 = CIRCLE ( 'NONE', #4971, 0.9000000000000003553 ) ;
#2664 = CARTESIAN_POINT ( 'NONE',  ( 32.75517961154501023, -5.344437665069116328, -7.939653947423664704 ) ) ;
#2665 = CARTESIAN_POINT ( 'NONE',  ( 31.89397184978405519, -6.712334120981523711, 5.783357778048664244 ) ) ;
#2666 = CARTESIAN_POINT ( 'NONE',  ( 4.000000000000000000, -0.8577736050348414576, -3.133260139357120888 ) ) ;
#2667 = CIRCLE ( 'NONE', #7875, 25.00000000000000000 ) ;
#2668 = CARTESIAN_POINT ( 'NONE',  ( 25.93488947238681774, -5.606027099510431988, -7.939653947423663816 ) ) ;
#2669 = AXIS2_PLACEMENT_3D ( 'NONE', #11406, #1553, #12604 ) ;
#2670 = ADVANCED_FACE ( 'NONE', ( #3837 ), #994, .F. ) ;
#2671 = CARTESIAN_POINT ( 'NONE',  ( 24.43282520912215006, -22.30499949230690504, -14.60822674442184699 ) ) ;
#2672 = CARTESIAN_POINT ( 'NONE',  ( 30.93831368681553684, -6.190304661545915188, 6.861505862736157368 ) ) ;
#2673 = LINE ( 'NONE', #1231, #1763 ) ;
#2674 = CARTESIAN_POINT ( 'NONE',  ( -4.197393957002304887, 0.4069871074557444013, -3.203767560748928211 ) ) ;
#2675 = ORIENTED_EDGE ( 'NONE', *, *, #6372, .T. ) ;
#2676 = AXIS2_PLACEMENT_3D ( 'NONE', #16925, #5738, #17108 ) ;
#2677 = CARTESIAN_POINT ( 'NONE',  ( 32.61569110240115776, -6.288022587442930522, -7.033357778048666908 ) ) ;
#2678 = VECTOR ( 'NONE', #9218, 1000.000000000000000 ) ;
#2679 = ORIENTED_EDGE ( 'NONE', *, *, #340, .F. ) ;
#2680 = CARTESIAN_POINT ( 'NONE',  ( 8.632250723006720250, -18.84644399697197770, 16.84735068286506987 ) ) ;
#2681 = DIRECTION ( 'NONE',  ( 0.000000000000000000, 0.000000000000000000, -1.000000000000000000 ) ) ;
#2682 = CARTESIAN_POINT ( 'NONE',  ( 29.15206445563513071, -6.405512418264540209, -6.861505862736167138 ) ) ;
#2683 = FACE_OUTER_BOUND ( 'NONE', #5573, .T. ) ;
#2684 = AXIS2_PLACEMENT_3D ( 'NONE', #253, #10021, #16757 ) ;
#2685 = DIRECTION ( 'NONE',  ( -1.000000000000000000, -1.501955125927555231E-12, 0.000000000000000000 ) ) ;
#2686 = CARTESIAN_POINT ( 'NONE',  ( 0.000000000000000000, 0.000000000000000000, 0.000000000000000000 ) ) ;
#2687 = LINE ( 'NONE', #9306, #4025 ) ;
#2688 = CARTESIAN_POINT ( 'NONE',  ( 28.14933959732260149, -3.391468297350501260, 3.627061608673666893 ) ) ;
#2689 = VECTOR ( 'NONE', #14563, 1000.000000000000000 ) ;
#2690 = EDGE_CURVE ( 'NONE', #6877, #15184, #9894, .T. ) ;
#2691 = CARTESIAN_POINT ( 'NONE',  ( 10.50000000000000000, 1.285879139104720831E-15, -4.000000000000000000 ) ) ;
#2692 = CARTESIAN_POINT ( 'NONE',  ( 25.71748644841968456, -2.420320648352046078, -5.783357778048663356 ) ) ;
#2693 = CARTESIAN_POINT ( 'NONE',  ( 32.19919549706052209, -6.038393303862174655, 6.861505862736157368 ) ) ;
#2694 = AXIS2_PLACEMENT_3D ( 'NONE', #17204, #949, #3586 ) ;
#2695 = ORIENTED_EDGE ( 'NONE', *, *, #4529, .F. ) ;
#2696 = ORIENTED_EDGE ( 'NONE', *, *, #6303, .T. ) ;
#2697 = ADVANCED_FACE ( 'NONE', ( #10867 ), #8084, .T. ) ;
#2698 = CARTESIAN_POINT ( 'NONE',  ( 31.28415083292585663, -5.521667582366822202, 7.939653947423658487 ) ) ;
#2699 = AXIS2_PLACEMENT_3D ( 'NONE', #13941, #7069, #164 ) ;
#2700 = DIRECTION ( 'NONE',  ( 0.9928203230275512992, 0.1196152422706610180, 4.006172263299093133E-17 ) ) ;
#2701 = EDGE_CURVE ( 'NONE', #6328, #3112, #1520, .T. ) ;
#2702 = VERTEX_POINT ( 'NONE', #8345 ) ;
#2703 = CARTESIAN_POINT ( 'NONE',  ( 28.26310972651430120, -2.123820177930694442, 5.783357778048668685 ) ) ;
#2704 = PRODUCT_RELATED_PRODUCT_CATEGORY ( 'part', '', ( #3615 ) ) ;
#2705 = CARTESIAN_POINT ( 'NONE',  ( 45.00000000000000711, -19.03270077640483038, 5.537981825772250843 ) ) ;
#2706 = DIRECTION ( 'NONE',  ( -1.000000000000000000, 0.000000000000000000, 0.000000000000000000 ) ) ;
#2707 = CARTESIAN_POINT ( 'NONE',  ( 32.92264866086529906, -1.552240892477451784, -6.453230759126466154 ) ) ;
#2708 = CARTESIAN_POINT ( 'NONE',  ( 26.37178701114681800, -2.351687214456304353, -5.783357778048658027 ) ) ;
#2709 = FACE_OUTER_BOUND ( 'NONE', #4089, .T. ) ;
#2710 = ORIENTED_EDGE ( 'NONE', *, *, #2456, .T. ) ;
#2711 = CARTESIAN_POINT ( 'NONE',  ( 29.89119874204131122, -2.254829357712824667, -4.533357778048659803 ) ) ;
#2712 = CARTESIAN_POINT ( 'NONE',  ( 31.98525019727866692, -6.363978266284800789, 4.533357778048659803 ) ) ;
#2713 = CARTESIAN_POINT ( 'NONE',  ( 32.60321786976872005, -6.626883982076972046, -5.783357778048663356 ) ) ;
#2714 = CARTESIAN_POINT ( 'NONE',  ( 0.000000000000000000, 0.000000000000000000, -6.000000000000000000 ) ) ;
#2715 = SHAPE_REPRESENTATION_RELATIONSHIP ( 'NONE' , 'NONE' ,  #12598, #7018 ) ;
#2716 = ORIENTED_EDGE ( 'NONE', *, *, #10180, .F. ) ;
#2717 = EDGE_CURVE ( 'NONE', #11807, #11418, #4188, .T. ) ;
#2718 = CARTESIAN_POINT ( 'NONE',  ( 28.93739072872572393, -3.296523698798161650, -7.939653947423660263 ) ) ;
#2719 = CARTESIAN_POINT ( 'NONE',  ( 30.19827253897071273, -3.144612341114421561, -7.939653947423660263 ) ) ;
#2720 = VERTEX_POINT ( 'NONE', #12425 ) ;
#2721 = CARTESIAN_POINT ( 'NONE',  ( 26.18940075748478691, -6.337263906362392341, 3.743184633113769699 ) ) ;
#2722 = CARTESIAN_POINT ( 'NONE',  ( 30.00264913441657555, -6.940201157507134511, 5.783357778048669573 ) ) ;
#2723 = ORIENTED_EDGE ( 'NONE', *, *, #17198, .T. ) ;
#2724 = ORIENTED_EDGE ( 'NONE', *, *, #11261, .T. ) ;
#2725 = CARTESIAN_POINT ( 'NONE',  ( 33.17094678975809074, -2.159493266760871499, 4.705209693361167567 ) ) ;
#2726 = CARTESIAN_POINT ( 'NONE',  ( 28.35948656569676629, -3.366149737736551906, -3.627061608673662896 ) ) ;
#2727 = DIRECTION ( 'NONE',  ( 0.5661261679878573094, 0.8243186046180107640, -0.000000000000000000 ) ) ;
#2728 = CARTESIAN_POINT ( 'NONE',  ( 45.50000000000000000, -16.03270077640482683, 5.537981825772250843 ) ) ;
#2729 = CYLINDRICAL_SURFACE ( 'NONE', #14532, 14.00000000000000178 ) ;
#2730 = CARTESIAN_POINT ( 'NONE',  ( 28.73594040535616756, -2.066853418799292630, -5.783357778048658027 ) ) ;
#2731 = DIRECTION ( 'NONE',  ( 1.000000000000000000, 0.000000000000000000, 0.000000000000000000 ) ) ;
#2732 = CYLINDRICAL_SURFACE ( 'NONE', #12468, 13.00000000000000178 ) ;
#2733 = CYLINDRICAL_SURFACE ( 'NONE', #360, 2.500000000000000000 ) ;
#2734 = CARTESIAN_POINT ( 'NONE',  ( 27.87986455999572399, -6.131689368163069531, -3.283357778048667797 ) ) ;
#2735 =( BOUNDED_CURVE ( )  B_SPLINE_CURVE ( 2, ( #17460, #9085, #12978, #14627, #14351, #5983, #14711, #17269, #10247 ),
 .UNSPECIFIED., .F., .F. ) 
 B_SPLINE_CURVE_WITH_KNOTS ( ( 3, 2, 2, 2, 3 ),
 ( 0.4807692307692307820, 0.4871794871794871695, 0.5000000000000000000, 0.5128205128205127750, 0.5192307692307692735 ),
 .UNSPECIFIED. ) 
 CURVE ( )  GEOMETRIC_REPRESENTATION_ITEM ( )  RATIONAL_B_SPLINE_CURVE ( ( 0.9330127018922194093, 0.9330127018922196314, 1.000000000000000000, 0.8660254037844387076, 1.000000000000000000, 0.8660254037844387076, 1.000000000000000000, 0.9330127018922187432, 0.9330127018922192983 ) ) 
 REPRESENTATION_ITEM ( '' )  );
#2736 = ORIENTED_EDGE ( 'NONE', *, *, #12430, .T. ) ;
#2737 = DIRECTION ( 'NONE',  ( 1.000000000000000000, 0.000000000000000000, 0.000000000000000000 ) ) ;
#2738 = CYLINDRICAL_SURFACE ( 'NONE', #11178, 2.499999999999999112 ) ;
#2739 = B_SPLINE_CURVE_WITH_KNOTS ( 'NONE', 3,
 ( #10555, #2068, #17409, #12011, #16120, #3680 ),
 .UNSPECIFIED., .F., .F.,
 ( 4, 2, 4 ),
 ( -3.640115492410573777E-06, 0.0002066546034006518627, 0.0004169493222937142949 ),
 .UNSPECIFIED. ) ;
#2740 = CARTESIAN_POINT ( 'NONE',  ( 4.281152949374537720, 4.203775615332211224, -3.000000000000000888 ) ) ;
#2741 = LINE ( 'NONE', #8262, #13559 ) ;
#2742 = EDGE_CURVE ( 'NONE', #11992, #7755, #15417, .T. ) ;
#2743 = CARTESIAN_POINT ( 'NONE',  ( 28.36401332423200827, -6.500457016816879374, -6.861505862736166250 ) ) ;
#2744 = EDGE_LOOP ( 'NONE', ( #16538, #8104, #960, #8680, #3077, #3144 ) ) ;
#2745 = CARTESIAN_POINT ( 'NONE',  ( -27.17934203385504333, -30.00000000000000355, 12.00000000000000000 ) ) ;
#2746 = DIRECTION ( 'NONE',  ( 0.000000000000000000, 0.000000000000000000, 1.000000000000000000 ) ) ;
#2747 = ORIENTED_EDGE ( 'NONE', *, *, #3548, .F. ) ;
#2748 = DIRECTION ( 'NONE',  ( 0.000000000000000000, 0.000000000000000000, 1.000000000000000000 ) ) ;
#2749 = ORIENTED_EDGE ( 'NONE', *, *, #16433, .F. ) ;
#2750 = PRODUCT_DEFINITION_SHAPE ( 'NONE', 'NONE',  #17970 ) ;
#2751 = CARTESIAN_POINT ( 'NONE',  ( 30.29464937815318493, -4.386941900920275472, -7.939653947423662039 ) ) ;
#2752 = DIRECTION ( 'NONE',  ( 0.000000000000000000, 0.000000000000000000, -1.000000000000000000 ) ) ;
#2753 = ORIENTED_EDGE ( 'NONE', *, *, #8666, .T. ) ;
#2754 = CARTESIAN_POINT ( 'NONE',  ( 25.96969170380761582, -2.000386719721422235, -5.783357778048658027 ) ) ;
#2755 = DIRECTION ( 'NONE',  ( 1.000000000000000000, 0.000000000000000000, -0.000000000000000000 ) ) ;
#2756 = DIRECTION ( 'NONE',  ( 0.000000000000000000, -1.000000000000000000, 0.000000000000000000 ) ) ;
#2757 = CARTESIAN_POINT ( 'NONE',  ( 27.75966235412334981, -2.811446176820259879, -4.705209693361160461 ) ) ;
#2758 = ADVANCED_FACE ( 'NONE', ( #11129 ), #4407, .T. ) ;
#2759 = ORIENTED_EDGE ( 'NONE', *, *, #9974, .T. ) ;
#2760 = CARTESIAN_POINT ( 'NONE',  ( 20.27597925817430635, -21.85809165190032743, -15.46244260681514326 ) ) ;
#2761 = VERTEX_POINT ( 'NONE', #1202 ) ;
#2762 = EDGE_CURVE ( 'NONE', #6838, #4560, #13379, .T. ) ;
#2763 = LINE ( 'NONE', #2936, #2828 ) ;
#2764 = SURFACE_STYLE_USAGE ( .BOTH. , #8017 ) ;
#2765 = CARTESIAN_POINT ( 'NONE',  ( 19.23308179030308551, -21.22208063239337505, 15.64628783324453387 ) ) ;
#2766 = ORIENTED_EDGE ( 'NONE', *, *, #17392, .F. ) ;
#2767 = VERTEX_POINT ( 'NONE', #15327 ) ;
#2768 = DIRECTION ( 'NONE',  ( -0.000000000000000000, -0.000000000000000000, 1.000000000000000000 ) ) ;
#2769 = EDGE_CURVE ( 'NONE', #14246, #7494, #9602, .T. ) ;
#2770 = ORIENTED_EDGE ( 'NONE', *, *, #14348, .F. ) ;
#2771 = CARTESIAN_POINT ( 'NONE',  ( 33.78529456515154550, -6.484467084455914687, -5.783357778048663356 ) ) ;
#2772 = CARTESIAN_POINT ( 'NONE',  ( 28.91999743871649997, -5.806501378023834370, -3.627061608673668225 ) ) ;
#2773 = CARTESIAN_POINT ( 'NONE',  ( -4.141042022537586575, 2.227970427079376758, -3.387027626239164313 ) ) ;
#2774 = CARTESIAN_POINT ( 'NONE',  ( 28.36392410707646761, -4.619556167269785796, -3.283357778048664688 ) ) ;
#2775 = CARTESIAN_POINT ( 'NONE',  ( 31.17093069310692499, -6.462087684996337345, -4.533357778048668685 ) ) ;
#2776 = CARTESIAN_POINT ( 'NONE',  ( 30.02326902268086428, -5.673578940050561847, 7.939653947423658487 ) ) ;
#2777 = CARTESIAN_POINT ( 'NONE',  ( 6.935828204433864386, -17.68137362934027124, 16.94363565911716663 ) ) ;
#2778 = CARTESIAN_POINT ( 'NONE',  ( 26.01595305975170547, -2.384361315936983416, -5.783357778048670461 ) ) ;
#2779 = CARTESIAN_POINT ( 'NONE',  ( 32.91278983782564183, -5.325448745358647429, 3.627061608673662896 ) ) ;
#2780 = ORIENTED_EDGE ( 'NONE', *, *, #13626, .F. ) ;
#2781 = VERTEX_POINT ( 'NONE', #2740 ) ;
#2782 = CARTESIAN_POINT ( 'NONE',  ( 26.88845778707760914, -3.543379655034240905, 3.627061608673666893 ) ) ;
#2783 = CARTESIAN_POINT ( 'NONE',  ( 28.53771668024168662, -2.080538600569502794, -5.783357778048658027 ) ) ;
#2784 = VERTEX_POINT ( 'NONE', #13973 ) ;
#2785 = CARTESIAN_POINT ( 'NONE',  ( 26.82722439997946395, -4.804698134550569044, 7.939653947423662039 ) ) ;
#2786 = CARTESIAN_POINT ( 'NONE',  ( 2.500000000000000000, -1.178949249685213863, 2.042000000000001148 ) ) ;
#2787 = CARTESIAN_POINT ( 'NONE',  ( -7.499998387031003411, -20.49508120620799900, 6.000000000000000000 ) ) ;
#2788 = ADVANCED_FACE ( 'NONE', ( #9518 ), #16296, .F. ) ;
#2789 = DIRECTION ( 'NONE',  ( -0.9979201627913402151, 0.06446199418653550395, 5.311609029246448998E-22 ) ) ;
#2790 = CARTESIAN_POINT ( 'NONE',  ( 26.85044460880409645, -7.319979551716484067, -5.783357778048668685 ) ) ;
#2791 = CARTESIAN_POINT ( 'NONE',  ( 28.52524344760924180, -2.419399995203538101, -7.033357778048658027 ) ) ;
#2792 = DIRECTION ( 'NONE',  ( -1.000000000000000000, 0.000000000000000000, 0.000000000000000000 ) ) ;
#2793 = CARTESIAN_POINT ( 'NONE',  ( -11.54660026683835383, -4.788112600790469742, -10.47749643873921244 ) ) ;
#2794 = CARTESIAN_POINT ( 'NONE',  ( 26.01652455409633902, -4.902371455920926380, 5.783357778048663356 ) ) ;
#2795 = CARTESIAN_POINT ( 'NONE',  ( 29.03376756790819613, -4.538853258604016006, -7.939653947423662039 ) ) ;
#2796 = CARTESIAN_POINT ( 'NONE',  ( 28.39010325924584421, -2.735490497978389612, -4.705209693361160461 ) ) ;
#2797 = CARTESIAN_POINT ( 'NONE',  ( 30.68374079916737429, -6.858143062403621926, -5.113484796970860558 ) ) ;
#2798 = CARTESIAN_POINT ( 'NONE',  ( -1.500000000000000222, -9.718191103688257115, -2.333127728361105824 ) ) ;
#2799 = ORIENTED_EDGE ( 'NONE', *, *, #11369, .T. ) ;
#2800 = ORIENTED_EDGE ( 'NONE', *, *, #3515, .F. ) ;
#2801 = EDGE_LOOP ( 'NONE', ( #3087, #14366, #10262, #4581, #2416, #1972 ) ) ;
#2802 = CARTESIAN_POINT ( 'NONE',  ( 32.64557936882268052, -2.222789665795767089, 6.861505862736165362 ) ) ;
#2803 = CARTESIAN_POINT ( 'NONE',  ( 30.98067518586950442, -1.786210345264705790, 5.783357778048667797 ) ) ;
#2804 = DIRECTION ( 'NONE',  ( 0.6000000000000001998, 0.7999999999999999334, 0.000000000000000000 ) ) ;
#2805 = CARTESIAN_POINT ( 'NONE',  ( 32.21340264088064487, -1.637691031382005669, -6.453230759126468818 ) ) ;
#2806 = EDGE_CURVE ( 'NONE', #13908, #625, #6456, .T. ) ;
#2807 = DIRECTION ( 'NONE',  ( -1.000000000000000000, 0.000000000000000000, 0.000000000000000000 ) ) ;
#2808 = CARTESIAN_POINT ( 'NONE',  ( 28.14933959732260149, -3.391468297350501260, -7.939653947423660263 ) ) ;
#2809 = CARTESIAN_POINT ( 'NONE',  ( 28.43075721014566781, -2.093425104433228157, -6.453230759126469707 ) ) ;
#2810 = ADVANCED_FACE ( 'NONE', ( #16359 ), #3920, .F. ) ;
#2811 = DIRECTION ( 'NONE',  ( -0.1196152422706610735, 0.9928203230275511881, 0.000000000000000000 ) ) ;
#2812 = CARTESIAN_POINT ( 'NONE',  ( 26.55511561737958814, -2.656761491791831187, -7.033357778048658027 ) ) ;
#2813 = VERTEX_POINT ( 'NONE', #5528 ) ;
#2814 = CARTESIAN_POINT ( 'NONE',  ( 30.75425665345519732, -2.450656702321377001, -4.705209693361161349 ) ) ;
#2815 = CARTESIAN_POINT ( 'NONE',  ( 2.500000000000000000, -1.178949249685213863, 2.042000000000001148 ) ) ;
#2816 = CARTESIAN_POINT ( 'NONE',  ( 5.200000000000002842, 0.000000000000000000, -2.700000000000000622 ) ) ;
#2817 = CARTESIAN_POINT ( 'NONE',  ( -0.02511946470933618461, 4.877415451931360835, -3.451298686683626826 ) ) ;
#2818 = CARTESIAN_POINT ( 'NONE',  ( 31.17093069310692499, -6.462087684996337345, -4.533357778048668685 ) ) ;
#2819 = AXIS2_PLACEMENT_3D ( 'NONE', #9984, #10346, #6188 ) ;
#2820 = CARTESIAN_POINT ( 'NONE',  ( 28.56093688906631911, -4.595820017735426255, -3.627061608673664672 ) ) ;
#2821 = EDGE_LOOP ( 'NONE', ( #11159, #16274, #16071, #4011, #2554 ) ) ;
#2822 = CARTESIAN_POINT ( 'NONE',  ( 26.31556265977298992, -7.384422263489805793, -5.783357778048663356 ) ) ;
#2823 = CARTESIAN_POINT ( 'NONE',  ( 2.749999999999988454, -20.49999999999999645, -13.00000000000000355 ) ) ;
#2824 = ORIENTED_EDGE ( 'NONE', *, *, #13327, .F. ) ;
#2825 = DIRECTION ( 'NONE',  ( 0.000000000000000000, 0.000000000000000000, 1.000000000000000000 ) ) ;
#2826 = ORIENTED_EDGE ( 'NONE', *, *, #13713, .T. ) ;
#2827 = EDGE_CURVE ( 'NONE', #4229, #11393, #12106, .T. ) ;
#2828 = VECTOR ( 'NONE', #2841, 1000.000000000000000 ) ;
#2829 = CARTESIAN_POINT ( 'NONE',  ( 31.56875459193803124, -6.114348982704044921, -4.705209693361169343 ) ) ;
#2830 = CARTESIAN_POINT ( 'NONE',  ( 29.39282811755836633, -5.749534618892433002, -3.627061608673667781 ) ) ;
#2831 = EDGE_CURVE ( 'NONE', #16316, #7502, #3825, .T. ) ;
#2832 = DIRECTION ( 'NONE',  ( 1.000000000000000000, 0.000000000000000000, 0.000000000000000000 ) ) ;
#2833 = CARTESIAN_POINT ( 'NONE',  ( 2.000000000000006217, 3.464101615137751722, -1.401678602859870442E-15 ) ) ;
#2834 = AXIS2_PLACEMENT_3D ( 'NONE', #16697, #7184, #7369 ) ;
#2835 = CARTESIAN_POINT ( 'NONE',  ( 28.52162355051263987, -6.481468097106410475, -6.861505862736167138 ) ) ;
#2836 = CARTESIAN_POINT ( 'NONE',  ( 28.55151181693415907, -2.416235175459247486, 7.033357778048666020 ) ) ;
#2837 = ORIENTED_EDGE ( 'NONE', *, *, #804, .T. ) ;
#2838 = VECTOR ( 'NONE', #13263, 1000.000000000000114 ) ;
#2839 = VERTEX_POINT ( 'NONE', #3278 ) ;
#2840 = AXIS2_PLACEMENT_3D ( 'NONE', #10627, #5283, #6394 ) ;
#2841 = DIRECTION ( 'NONE',  ( -1.000000000000000000, 0.000000000000000000, 0.000000000000000000 ) ) ;
#2842 = CARTESIAN_POINT ( 'NONE',  ( -24.42841412577760352, -22.30604244805903136, 14.60923613736931514 ) ) ;
#2843 = CARTESIAN_POINT ( 'NONE',  ( 33.24613200752366282, -6.212066908601060256, 4.533357778048659803 ) ) ;
#2844 = ORIENTED_EDGE ( 'NONE', *, *, #3254, .T. ) ;
#2845 = CARTESIAN_POINT ( 'NONE',  ( 31.26353094466156080, -6.788289799823394866, 5.783357778048664244 ) ) ;
#2846 = ORIENTED_EDGE ( 'NONE', *, *, #17557, .T. ) ;
#2847 = CARTESIAN_POINT ( 'NONE',  ( 27.29063000668916672, -2.568146533142987575, -4.533357778048659803 ) ) ;
#2848 = EDGE_CURVE ( 'NONE', #3354, #5056, #4954, .T. ) ;
#2849 =( BOUNDED_SURFACE ( )  B_SPLINE_SURFACE ( 1, 2, ( 
 ( #11911, #9285, #14827, #17586, #13375, #957, #7848, #16199, #5106, #3764, #10626, #12005, #6490, #260, #11285, #7070, #2984, #11387, #8785, #11191, #16862, #9938, #13942, #4511, #9750, #448, #10027, #7157, #4426, #12861, #1536, #16955, #15575, #5950, #11474, #17042, #15488, #4249, #12587, #10118, #12667, #166, #3070, #4333, #15302, #15669, #5770, #8590, #5677, #8505, #3154, #14318, #16762, #14125, #1713, #9845, #8690, #2883, #4597, #14219, #7245, #1813, #15397, #7342, #3249, #14040, #6964, #12494, #1627, #12761, #8410, #356, #5864, #81, #5590, #16675, #11107, #9137, #13129, #10216, #5044, #11843, #14495, #4775, #6142, #620, #4689, #9046, #10566, #15765, #13217, #16130, #17236, #16046, #3338, #11752, #11934, #4952, #793, #6321, #14599, #17420, #11571, #3692, #10298, #6416, #10481, #15944, #707, #2174, #9217, #17321, #11668, #3614, #1901, #15849, #527, #14675, #2256, #8869, #7773, #13302, #884, #14402, #17523, #3423, #7426, #12941, #1985, #7689, #6042, #17139, #2080, #7508, #13031, #4862, #8954, #7603, #6232, #3514, #10391, #10229, #8969, #7526, #1826, #7358, #14332, #8800, #15777, #6157, #1728, #1915, #5879 ),
 ( #3084, #14512, #632, #4612, #7258, #2095, #3351, #5963, #14237, #15589, #10041, #14138, #541, #7619, #12776, #4702, #13142, #8705, #13047, #372, #3265, #3439, #14418, #8884, #2000, #6056, #11681, #8606, #721, #12875, #15867, #17251, #7437, #10136, #11585, #11300, #12957, #3166, #4790, #16879, #460, #9952, #10310, #4441, #11403, #15503, #16967, #4524, #11489, #17058, #15684, #17153, #17623, #9062, #998, #13588, #1076, #6433, #13228, #6599, #16146, #15963, #10499, #11860, #2367, #3889, #9230, #901, #13503, #14860, #11956, #3707, #6523, #5229, #14609, #2273, #17439, #12129, #2187, #14779, #17538, #7884, #17709, #806, #16232, #3805, #10751, #16327, #9404, #10579, #3530, #6336, #14946, #5058, #4970, #13417, #3630, #7702, #2523, #12035, #5142, #16060, #7791, #10660, #8050, #9152, #9321, #2448, #14691, #7971, #13321, #6246, #11767, #17340, #4878, #10408, #16669, #5672, #15121, #11183, #7060, #4059, #6954, #15028, #5492, #16756, #12486, #15208, #17960, #8312, #4327, #16575, #17879, #5584, #2976, #2708, #17798, #4241, #13935, #2616, #11101, #1530, #160, #13675, #15295, #5402, #72, #9741, #3974, #13844, #8499, #12579, #1341 ) ),
 .UNSPECIFIED., .F., .F., .T. ) 
 B_SPLINE_SURFACE_WITH_KNOTS ( ( 2, 2 ),
 ( 3, 2, 2, 2, 2, 2, 2, 2, 2, 2, 2, 2, 2, 2, 2, 2, 2, 2, 2, 2, 2, 2, 2, 2, 2, 2, 2, 2, 2, 2, 2, 2, 2, 2, 2, 2, 2, 2, 2, 2, 2, 2, 2, 2, 2, 2, 2, 2, 2, 2, 2, 2, 2, 2, 2, 2, 2, 2, 2, 2, 2, 2, 2, 2, 2, 2, 2, 2, 2, 2, 2, 2, 2, 2, 2, 2, 3 ),
 ( 0.000000000000000000, 1.000000000000000000 ),
 ( 0.000000000000000000, 0.01282051282051282007, 0.02564102564102564014, 0.03846153846153846367, 0.05128205128205128027, 0.06410256410256409687, 0.07692307692307692735, 0.08974358974358974395, 0.1025641025641025605, 0.1153846153846153910, 0.1282051282051281937, 0.1410256410256410242, 0.1538461538461538547, 0.1666666666666666574, 0.1794871794871794879, 0.1923076923076923184, 0.2051282051282051211, 0.2179487179487179516, 0.2307692307692307820, 0.2435897435897435848, 0.2564102564102563875, 0.2692307692307692180, 0.2820512820512820484, 0.2948717948717948789, 0.3076923076923077094, 0.3205128205128205399, 0.3333333333333333148, 0.3461538461538461453, 0.3589743589743589758, 0.3717948717948718063, 0.3846153846153846367, 0.3974358974358974117, 0.4102564102564102422, 0.4230769230769230727, 0.4358974358974359031, 0.4487179487179487336, 0.4615384615384615641, 0.4743589743589743390, 0.4871794871794871695, 0.5000000000000000000, 0.5128205128205127750, 0.5256410256410256610, 0.5384615384615384359, 0.5512820512820513219, 0.5641025641025640969, 0.5769230769230768718, 0.5897435897435897578, 0.6025641025641025328, 0.6153846153846154188, 0.6282051282051281937, 0.6410256410256410797, 0.6538461538461538547, 0.6666666666666666297, 0.6794871794871795156, 0.6923076923076922906, 0.7051282051282051766, 0.7179487179487179516, 0.7307692307692307265, 0.7435897435897436125, 0.7564102564102563875, 0.7692307692307692735, 0.7820512820512820484, 0.7948717948717948234, 0.8076923076923077094, 0.8205128205128204844, 0.8333333333333333703, 0.8461538461538461453, 0.8589743589743589203, 0.8717948717948718063, 0.8846153846153845812, 0.8974358974358974672, 0.9102564102564102422, 0.9230769230769231282, 0.9358974358974359031, 0.9487179487179486781, 0.9615384615384615641, 0.9690838366659333403 ),
 .UNSPECIFIED. ) 
 GEOMETRIC_REPRESENTATION_ITEM ( )  RATIONAL_B_SPLINE_SURFACE ( (
 ( 1.000000000000000000, 0.8660254037844387076, 1.000000000000000000, 0.8660254037844387076, 1.000000000000000000, 0.8660254037844387076, 1.000000000000000000, 0.8660254037844387076, 1.000000000000000000, 0.8660254037844387076, 1.000000000000000000, 0.8660254037844387076, 1.000000000000000000, 0.8660254037844387076, 1.000000000000000000, 0.8660254037844387076, 1.000000000000000000, 0.8660254037844387076, 1.000000000000000000, 0.8660254037844387076, 1.000000000000000000, 0.8660254037844387076, 1.000000000000000000, 0.8660254037844387076, 1.000000000000000000, 0.8660254037844387076, 1.000000000000000000, 0.8660254037844387076, 1.000000000000000000, 0.8660254037844387076, 1.000000000000000000, 0.8660254037844387076, 1.000000000000000000, 0.8660254037844387076, 1.000000000000000000, 0.8660254037844387076, 1.000000000000000000, 0.8660254037844387076, 1.000000000000000000, 0.8660254037844387076, 1.000000000000000000, 0.8660254037844387076, 1.000000000000000000, 0.8660254037844387076, 1.000000000000000000, 0.8660254037844387076, 1.000000000000000000, 0.8660254037844387076, 1.000000000000000000, 0.8660254037844387076, 1.000000000000000000, 0.8660254037844387076, 1.000000000000000000, 0.8660254037844387076, 1.000000000000000000, 0.8660254037844387076, 1.000000000000000000, 0.8660254037844387076, 1.000000000000000000, 0.8660254037844387076, 1.000000000000000000, 0.8660254037844387076, 1.000000000000000000, 0.8660254037844387076, 1.000000000000000000, 0.8660254037844387076, 1.000000000000000000, 0.8660254037844387076, 1.000000000000000000, 0.8660254037844387076, 1.000000000000000000, 0.8660254037844387076, 1.000000000000000000, 0.8660254037844387076, 1.000000000000000000, 0.8660254037844387076, 1.000000000000000000, 0.8660254037844387076, 1.000000000000000000, 0.8660254037844387076, 1.000000000000000000, 0.8660254037844387076, 1.000000000000000000, 0.8660254037844387076, 1.000000000000000000, 0.8660254037844387076, 1.000000000000000000, 0.8660254037844387076, 1.000000000000000000, 0.8660254037844387076, 1.000000000000000000, 0.8660254037844387076, 1.000000000000000000, 0.8660254037844387076, 1.000000000000000000, 0.8660254037844387076, 1.000000000000000000, 0.8660254037844387076, 1.000000000000000000, 0.8660254037844387076, 1.000000000000000000, 0.8660254037844387076, 1.000000000000000000, 0.8660254037844387076, 1.000000000000000000, 0.8660254037844387076, 1.000000000000000000, 0.8660254037844387076, 1.000000000000000000, 0.8660254037844387076, 1.000000000000000000, 0.8660254037844387076, 1.000000000000000000, 0.8660254037844387076, 1.000000000000000000, 0.8660254037844387076, 1.000000000000000000, 0.8660254037844387076, 1.000000000000000000, 0.8660254037844387076, 1.000000000000000000, 0.8660254037844387076, 1.000000000000000000, 0.8660254037844387076, 1.000000000000000000, 0.8660254037844387076, 1.000000000000000000, 0.8660254037844387076, 1.000000000000000000, 0.8660254037844387076, 1.000000000000000000, 0.8660254037844387076, 1.000000000000000000, 0.8660254037844387076, 1.000000000000000000, 0.8660254037844387076, 1.000000000000000000, 0.8660254037844387076, 1.000000000000000000, 0.8660254037844387076, 1.000000000000000000, 0.8660254037844387076, 1.000000000000000000, 0.8660254037844387076, 1.000000000000000000, 0.8660254037844387076, 1.000000000000000000, 0.8660254037844387076, 1.000000000000000000, 0.8660254037844387076, 1.000000000000000000, 0.9211506902921580142, 0.9351132093492240394),
 ( 1.000000000000000000, 0.8660254037844387076, 1.000000000000000000, 0.8660254037844387076, 1.000000000000000000, 0.8660254037844387076, 1.000000000000000000, 0.8660254037844387076, 1.000000000000000000, 0.8660254037844387076, 1.000000000000000000, 0.8660254037844387076, 1.000000000000000000, 0.8660254037844387076, 1.000000000000000000, 0.8660254037844387076, 1.000000000000000000, 0.8660254037844387076, 1.000000000000000000, 0.8660254037844387076, 1.000000000000000000, 0.8660254037844387076, 1.000000000000000000, 0.8660254037844387076, 1.000000000000000000, 0.8660254037844387076, 1.000000000000000000, 0.8660254037844387076, 1.000000000000000000, 0.8660254037844387076, 1.000000000000000000, 0.8660254037844387076, 1.000000000000000000, 0.8660254037844387076, 1.000000000000000000, 0.8660254037844387076, 1.000000000000000000, 0.8660254037844387076, 1.000000000000000000, 0.8660254037844387076, 1.000000000000000000, 0.8660254037844387076, 1.000000000000000000, 0.8660254037844387076, 1.000000000000000000, 0.8660254037844387076, 1.000000000000000000, 0.8660254037844387076, 1.000000000000000000, 0.8660254037844387076, 1.000000000000000000, 0.8660254037844387076, 1.000000000000000000, 0.8660254037844387076, 1.000000000000000000, 0.8660254037844387076, 1.000000000000000000, 0.8660254037844387076, 1.000000000000000000, 0.8660254037844387076, 1.000000000000000000, 0.8660254037844387076, 1.000000000000000000, 0.8660254037844387076, 1.000000000000000000, 0.8660254037844387076, 1.000000000000000000, 0.8660254037844387076, 1.000000000000000000, 0.8660254037844387076, 1.000000000000000000, 0.8660254037844387076, 1.000000000000000000, 0.8660254037844387076, 1.000000000000000000, 0.8660254037844387076, 1.000000000000000000, 0.8660254037844387076, 1.000000000000000000, 0.8660254037844387076, 1.000000000000000000, 0.8660254037844387076, 1.000000000000000000, 0.8660254037844387076, 1.000000000000000000, 0.8660254037844387076, 1.000000000000000000, 0.8660254037844387076, 1.000000000000000000, 0.8660254037844387076, 1.000000000000000000, 0.8660254037844387076, 1.000000000000000000, 0.8660254037844387076, 1.000000000000000000, 0.8660254037844387076, 1.000000000000000000, 0.8660254037844387076, 1.000000000000000000, 0.8660254037844387076, 1.000000000000000000, 0.8660254037844387076, 1.000000000000000000, 0.8660254037844387076, 1.000000000000000000, 0.8660254037844387076, 1.000000000000000000, 0.8660254037844387076, 1.000000000000000000, 0.8660254037844387076, 1.000000000000000000, 0.8660254037844387076, 1.000000000000000000, 0.8660254037844387076, 1.000000000000000000, 0.8660254037844387076, 1.000000000000000000, 0.8660254037844387076, 1.000000000000000000, 0.8660254037844387076, 1.000000000000000000, 0.8660254037844387076, 1.000000000000000000, 0.8660254037844387076, 1.000000000000000000, 0.8660254037844387076, 1.000000000000000000, 0.8660254037844387076, 1.000000000000000000, 0.8660254037844387076, 1.000000000000000000, 0.8660254037844387076, 1.000000000000000000, 0.8660254037844387076, 1.000000000000000000, 0.8660254037844387076, 1.000000000000000000, 0.8660254037844387076, 1.000000000000000000, 0.8660254037844387076, 1.000000000000000000, 0.8660254037844387076, 1.000000000000000000, 0.8660254037844387076, 1.000000000000000000, 0.8660254037844387076, 1.000000000000000000, 0.8660254037844387076, 1.000000000000000000, 0.8660254037844387076, 1.000000000000000000, 0.9211506902921580142, 0.9351132093492240394) ) ) 
 REPRESENTATION_ITEM ( '' )  SURFACE ( )  );
#2850 = ORIENTED_EDGE ( 'NONE', *, *, #3407, .T. ) ;
#2851 = CARTESIAN_POINT ( 'NONE',  ( 27.91310269393460430, -7.181753375802955475, -5.783357778048669573 ) ) ;
#2852 = VECTOR ( 'NONE', #15204, 1000.000000000000000 ) ;
#2853 = DIRECTION ( 'NONE',  ( 0.000000000000000000, -1.000000000000000000, 0.000000000000000000 ) ) ;
#2854 = CARTESIAN_POINT ( 'NONE',  ( 0.000000000000000000, 0.000000000000000000, 0.000000000000000000 ) ) ;
#2855 = CARTESIAN_POINT ( 'NONE',  ( 0.000000000000000000, 0.000000000000000000, 0.000000000000000000 ) ) ;
#2856 = FACE_OUTER_BOUND ( 'NONE', #10015, .T. ) ;
#2857 = EDGE_CURVE ( 'NONE', #1544, #9271, #1116, .T. ) ;
#2858 = CARTESIAN_POINT ( 'NONE',  ( 28.25893984004492765, -6.513116296623863377, 6.861505862736158257 ) ) ;
#2859 = DIRECTION ( 'NONE',  ( -0.9928203230275512992, -0.1196152422706610319, -9.614813431917826478E-17 ) ) ;
#2860 = DIRECTION ( 'NONE',  ( 0.9928203230275512992, 0.1196152422706610180, 4.006172263299093133E-17 ) ) ;
#2861 = CARTESIAN_POINT ( 'NONE',  ( 33.76207435632690590, -3.969185667289998332, 7.939653947423662039 ) ) ;
#2862 =( BOUNDED_CURVE ( )  B_SPLINE_CURVE ( 2, ( #15273, #10994, #17940, #11083, #2774, #6670, #8294, #8030, #16647 ),
 .UNSPECIFIED., .F., .T. ) 
 B_SPLINE_CURVE_WITH_KNOTS ( ( 3, 2, 2, 2, 3 ),
 ( 0.5961538461538461453, 0.6025641025641025328, 0.6153846153846154188, 0.6282051282051281937, 0.6346153846153846922 ),
 .UNSPECIFIED. ) 
 CURVE ( )  GEOMETRIC_REPRESENTATION_ITEM ( )  RATIONAL_B_SPLINE_CURVE ( ( 0.9330127018922194093, 0.9330127018922194093, 1.000000000000000000, 0.8660254037844387076, 1.000000000000000000, 0.8660254037844387076, 1.000000000000000000, 0.9330127018922187432, 0.9330127018922192983 ) ) 
 REPRESENTATION_ITEM ( '' )  );
#2863 = AXIS2_PLACEMENT_3D ( 'NONE', #2573, #8100, #5363 ) ;
#2864 = EDGE_LOOP ( 'NONE', ( #12798, #17774, #14164, #12910, #16398, #6826, #3386, #16138, #12474, #5065, #5356 ) ) ;
#2865 = ORIENTED_EDGE ( 'NONE', *, *, #16472, .T. ) ;
#2866 = VERTEX_POINT ( 'NONE', #8811 ) ;
#2867 = CARTESIAN_POINT ( 'NONE',  ( 28.38593337277646711, -7.124786616671554107, 5.783357778048658027 ) ) ;
#2868 = CARTESIAN_POINT ( 'NONE',  ( 8.776279441628840772, 6.799038105676637578, -11.72793873352922489 ) ) ;
#2869 = ORIENTED_EDGE ( 'NONE', *, *, #510, .F. ) ;
#2870 = CARTESIAN_POINT ( 'NONE',  ( 27.45766530510195835, -4.728742455708699666, 7.939653947423662039 ) ) ;
#2871 = ORIENTED_EDGE ( 'NONE', *, *, #7022, .F. ) ;
#2872 = ORIENTED_EDGE ( 'NONE', *, *, #3783, .T. ) ;
#2873 = DIRECTION ( 'NONE',  ( -0.8660254037844363761, 0.5000000000000038858, 0.000000000000000000 ) ) ;
#2874 = CARTESIAN_POINT ( 'NONE',  ( 23.00000000000000000, -16.21813761408365195, -13.00000000000000178 ) ) ;
#2875 = EDGE_LOOP ( 'NONE', ( #6703, #8241, #15202, #6122, #14011 ) ) ;
#2876 = CARTESIAN_POINT ( 'NONE',  ( 29.45101334415624095, -7.006662376286321603, 5.783357778048669573 ) ) ;
#2877 = FACE_OUTER_BOUND ( 'NONE', #11593, .T. ) ;
#2878 = DIRECTION ( 'NONE',  ( -0.1196152422706611984, 0.9928203230275510771, 0.000000000000000000 ) ) ;
#2879 = CARTESIAN_POINT ( 'NONE',  ( 30.66050125466253107, -2.889050389913576655, -3.283357778048662023 ) ) ;
#2880 = CARTESIAN_POINT ( 'NONE',  ( 32.29295089585318834, -5.599999616269981217, -3.283357778048667797 ) ) ;
#2881 = CARTESIAN_POINT ( 'NONE',  ( 26.29446227649215473, -10.90310086042137350, -14.16253947949896563 ) ) ;
#2882 = DIRECTION ( 'NONE',  ( 0.9928203230275510771, 0.1196152422706609902, 4.006172263299092517E-17 ) ) ;
#2883 = CARTESIAN_POINT ( 'NONE',  ( 30.90769699326644826, -6.820963901304073929, -5.783357778048668685 ) ) ;
#2884 = VECTOR ( 'NONE', #899, 1000.000000000000114 ) ;
#2885 = CARTESIAN_POINT ( 'NONE',  ( 29.66420847303068697, -4.462897579762144851, -7.939653947423662039 ) ) ;
#2886 = CARTESIAN_POINT ( 'NONE',  ( 30.71189515440122975, -6.854751018602581958, -5.783357778048663356 ) ) ;
#2887 = EDGE_CURVE ( 'NONE', #10072, #11560, #9139, .T. ) ;
#2888 = EDGE_LOOP ( 'NONE', ( #12997, #10963, #441, #14172 ) ) ;
#2889 = VERTEX_POINT ( 'NONE', #3617 ) ;
#2890 = VERTEX_POINT ( 'NONE', #12787 ) ;
#2891 = CARTESIAN_POINT ( 'NONE',  ( 29.64681518302145946, -6.972875258987813574, 5.783357778048658915 ) ) ;
#2892 = CYLINDRICAL_SURFACE ( 'NONE', #4161, 1.000000000000000000 ) ;
#2893 = VECTOR ( 'NONE', #5036, 1000.000000000000000 ) ;
#2894 = CARTESIAN_POINT ( 'NONE',  ( 25.81704846941310549, -3.246696919197674447, -4.409389677717624245 ) ) ;
#2895 = EDGE_CURVE ( 'NONE', #2890, #14870, #14678, .T. ) ;
#2896 = CARTESIAN_POINT ( 'NONE',  ( 29.99682221560115991, -1.914942061115552541, -5.783357778048658027 ) ) ;
#2897 = DIRECTION ( 'NONE',  ( 0.000000000000000000, 0.000000000000000000, -1.000000000000000000 ) ) ;
#2898 = DIRECTION ( 'NONE',  ( 0.6951637808321680101, -0.2969442527608454063, 0.6546536707079773088 ) ) ;
#2899 = CARTESIAN_POINT ( 'NONE',  ( 27.36943512155133362, -2.558652073080304845, -4.533357778048659803 ) ) ;
#2900 =( GEOMETRIC_REPRESENTATION_CONTEXT ( 3 ) GLOBAL_UNCERTAINTY_ASSIGNED_CONTEXT ( ( #12605 ) ) GLOBAL_UNIT_ASSIGNED_CONTEXT ( ( #13555, #12455, #3862 ) ) REPRESENTATION_CONTEXT ( 'NONE', 'WORKASPACE' ) );
#2901 = CARTESIAN_POINT ( 'NONE',  ( 27.45957062324739795, -6.182326487390973568, -8.283357778048662468 ) ) ;
#2902 = CARTESIAN_POINT ( 'NONE',  ( 30.23341599105502908, -5.648260380436597394, -7.939653947423664704 ) ) ;
#2903 = CARTESIAN_POINT ( 'NONE',  ( 28.21828588914510050, -7.155181690169023057, -6.453230759126468818 ) ) ;
#2904 = DIRECTION ( 'NONE',  ( 0.9928203230275512992, 0.1196152422706614898, -0.000000000000000000 ) ) ;
#2905 = CARTESIAN_POINT ( 'NONE',  ( 30.44283453230164227, -2.188368138933637574, 7.033357778048666020 ) ) ;
#2906 = CARTESIAN_POINT ( 'NONE',  ( 29.08935247050201767, -2.014077381790315702, 5.783357778048667797 ) ) ;
#2907 = ADVANCED_FACE ( 'NONE', ( #2259 ), #10051, .F. ) ;
#2908 = CARTESIAN_POINT ( 'NONE',  ( 31.84257795004535652, -2.746633492292519296, 8.283357778048664244 ) ) ;
#2909 = CARTESIAN_POINT ( 'NONE',  ( 30.15026255541241440, -6.285249260098253465, -4.705209693361168455 ) ) ;
#2910 = ORIENTED_EDGE ( 'NONE', *, *, #10359, .T. ) ;
#2911 = CIRCLE ( 'NONE', #9561, 2.749999999999991118 ) ;
#2912 = AXIS2_PLACEMENT_3D ( 'NONE', #5047, #6322, #3618 ) ;
#2913 = DIRECTION ( 'NONE',  ( -0.1196152422706610735, 0.9928203230275511881, 0.000000000000000000 ) ) ;
#2914 = CARTESIAN_POINT ( 'NONE',  ( -12.70000000000000284, 0.000000000000000000, 0.000000000000000000 ) ) ;
#2915 = VERTEX_POINT ( 'NONE', #7776 ) ;
#2916 = CARTESIAN_POINT ( 'NONE',  ( -25.76257153370368869, -10.59741316493651730, -14.29454127969954591 ) ) ;
#2917 = EDGE_CURVE ( 'NONE', #12636, #9205, #9827, .T. ) ;
#2918 = ORIENTED_EDGE ( 'NONE', *, *, #11232, .T. ) ;
#2919 = CARTESIAN_POINT ( 'NONE',  ( 30.81132015408399027, -5.578634341498224458, -3.627061608673668225 ) ) ;
#2920 = VERTEX_POINT ( 'NONE', #285 ) ;
#2921 = CARTESIAN_POINT ( 'NONE',  ( -9.480241546517731877, 0.6123889447720874957, -6.899999999999998579 ) ) ;
#2922 = ORIENTED_EDGE ( 'NONE', *, *, #10483, .F. ) ;
#2923 = ORIENTED_EDGE ( 'NONE', *, *, #1056, .T. ) ;
#2924 = CARTESIAN_POINT ( 'NONE',  ( 29.38830135902312080, -2.615227339812091767, -6.861505862736159145 ) ) ;
#2925 = LINE ( 'NONE', #209, #286 ) ;
#2926 = DIRECTION ( 'NONE',  ( 0.000000000000000000, 0.000000000000000000, -1.000000000000000000 ) ) ;
#2927 = CIRCLE ( 'NONE', #8724, 0.9999999999999995559 ) ;
#2928 = ORIENTED_EDGE ( 'NONE', *, *, #8053, .T. ) ;
#2929 = CARTESIAN_POINT ( 'NONE',  ( 33.32864623319426300, -4.021405196597508613, -3.283357778048664688 ) ) ;
#2930 = EDGE_CURVE ( 'NONE', #13090, #10047, #16789, .T. ) ;
#2931 = CARTESIAN_POINT ( 'NONE',  ( 17.31832318566733164, -18.83027996791590652, -15.95242868103980172 ) ) ;
#2932 = VERTEX_POINT ( 'NONE', #4358 ) ;
#2933 = CARTESIAN_POINT ( 'NONE',  ( 32.51858583609114106, -1.611119345748072362, 5.783357778048668685 ) ) ;
#2934 = VECTOR ( 'NONE', #4348, 1000.000000000000114 ) ;
#2935 =( BOUNDED_CURVE ( )  B_SPLINE_CURVE ( 2, ( #12242, #15140, #13520, #10938, #2725, #12409, #1278, #6799, #6538, #8247, #10854, #16422, #3820, #8068, #2802, #12051, #9337, #7985, #8162, #16504, #8327, #3988, #10675, #5246, #6616, #15047, #4175, #3907, #17813, #5512, #16347, #13605, #9504, #13694, #3688, #12327, #5331, #17638, #17892, #14877, #5423, #1093, #4075, #9674, #9585, #1357, #11030, #6880, #12146, #15225, #1013, #5158, #16249, #2464, #9419, #17726, #10766, #14958, #2543, #1188, #6704, #16770, #9853, #366, #15679, #175, #455, #12869, #11484, #1545, #16683, #7352, #11397, #15497, #5873, #7078, #16961, #5957, #10035, #12676, #5685, #2891, #4256, #17052, #14132, #4519, #4341, #1722, #8419, #4605, #15311, #13859, #1635, #15582, #4435, #15407, #11294, #11200, #7253, #90, #2993, #9757, #12770, #10129, #8515, #3258, #14048, #3161, #8599, #8699, #14232, #1820, #1447, #6975, #5597, #12505, #7167, #268, #11114, #13953, #5779, #12594, #16873, #9945, #3078, #6152, #1909, #13223, #10573, #13042, #13315, #7784, #6427, #14412, #11578, #2266, #6330, #10401, #800, #1994, #11851, #17246, #4871, #11947, #14685, #15771, #17148 ),
 .UNSPECIFIED., .F., .T. ) 
 B_SPLINE_CURVE_WITH_KNOTS ( ( 3, 2, 2, 2, 2, 2, 2, 2, 2, 2, 2, 2, 2, 2, 2, 2, 2, 2, 2, 2, 2, 2, 2, 2, 2, 2, 2, 2, 2, 2, 2, 2, 2, 2, 2, 2, 2, 2, 2, 2, 2, 2, 2, 2, 2, 2, 2, 2, 2, 2, 2, 2, 2, 2, 2, 2, 2, 2, 2, 2, 2, 2, 2, 2, 2, 2, 2, 2, 2, 2, 2, 2, 2, 3 ),
 ( 0.000000000000000000, 0.01322951968774666726, 0.02645903937549333451, 0.03968855906324000177, 0.05291807875098666902, 0.06614759843873332934, 0.07937711812648000353, 0.09260663781422667773, 0.1058361575019733380, 0.1190656771897200122, 0.1322951968774666587, 0.1455247165652133190, 0.1587542362529600071, 0.1719837559407066396, 0.1852132756284533555, 0.1984427953162000158, 0.2116723150039466761, 0.2249018346916933364, 0.2381313543794400245, 0.2513608740671866570, 0.2645903937549333174, 0.2778199134426800332, 0.2910494331304266380, 0.3042789528181733538, 0.3175084725059200141, 0.3307379921936667300, 0.3439675118814132793, 0.3571970315691599951, 0.3704265512569067109, 0.3836560709446533712, 0.3968855906324000316, 0.4101151103201466364, 0.4233446300078933522, 0.4365741496956400125, 0.4498036693833866728, 0.4630331890711333331, 0.4762627087588800490, 0.4894922284466267093, 0.5027217481343733141, 0.5159512678221199744, 0.5291807875098666347, 0.5424103071976132950, 0.5556398268853600664, 0.5688693465731067267, 0.5820988662608532760, 0.5953283859485999363, 0.6085579056363467076, 0.6217874253240932569, 0.6350169450118400283, 0.6482464646995866886, 0.6614759843873334599, 0.6747055040750800092, 0.6879350237628265585, 0.7011645434505734409, 0.7143940631383199902, 0.7276235828260666505, 0.7408531025138134218, 0.7540826222015599711, 0.7673121418893067425, 0.7805416615770532918, 0.7937711812648000631, 0.8070007009525467234, 0.8202302206402932727, 0.8334597403280399330, 0.8466892600157867044, 0.8599187797035333647, 0.8731482993912800250, 0.8863778190790266853, 0.8996073387667733456, 0.9128368584545200060, 0.9260663781422666663, 0.9392958978300133266, 0.9525254175177600979, 0.9555550897579921932 ),
 .UNSPECIFIED. ) 
 CURVE ( )  GEOMETRIC_REPRESENTATION_ITEM ( )  RATIONAL_B_SPLINE_CURVE ( ( 1.000000000000000000, 0.8660254037844387076, 1.000000000000000000, 0.8660254037844387076, 1.000000000000000000, 0.8660254037844387076, 1.000000000000000000, 0.8660254037844387076, 1.000000000000000000, 0.8660254037844387076, 1.000000000000000000, 0.8660254037844387076, 1.000000000000000000, 0.8660254037844387076, 1.000000000000000000, 0.8660254037844387076, 1.000000000000000000, 0.8660254037844387076, 1.000000000000000000, 0.8660254037844387076, 1.000000000000000000, 0.8660254037844387076, 1.000000000000000000, 0.8660254037844387076, 1.000000000000000000, 0.8660254037844387076, 1.000000000000000000, 0.8660254037844387076, 1.000000000000000000, 0.8660254037844387076, 1.000000000000000000, 0.8660254037844387076, 1.000000000000000000, 0.8660254037844387076, 1.000000000000000000, 0.8660254037844387076, 1.000000000000000000, 0.8660254037844387076, 1.000000000000000000, 0.8660254037844387076, 1.000000000000000000, 0.8660254037844387076, 1.000000000000000000, 0.8660254037844387076, 1.000000000000000000, 0.8660254037844387076, 1.000000000000000000, 0.8660254037844387076, 1.000000000000000000, 0.8660254037844387076, 1.000000000000000000, 0.8660254037844387076, 1.000000000000000000, 0.8660254037844387076, 1.000000000000000000, 0.8660254037844387076, 1.000000000000000000, 0.8660254037844387076, 1.000000000000000000, 0.8660254037844387076, 1.000000000000000000, 0.8660254037844387076, 1.000000000000000000, 0.8660254037844387076, 1.000000000000000000, 0.8660254037844387076, 1.000000000000000000, 0.8660254037844387076, 1.000000000000000000, 0.8660254037844387076, 1.000000000000000000, 0.8660254037844387076, 1.000000000000000000, 0.8660254037844387076, 1.000000000000000000, 0.8660254037844387076, 1.000000000000000000, 0.8660254037844387076, 1.000000000000000000, 0.8660254037844387076, 1.000000000000000000, 0.8660254037844387076, 1.000000000000000000, 0.8660254037844387076, 1.000000000000000000, 0.8660254037844387076, 1.000000000000000000, 0.8660254037844387076, 1.000000000000000000, 0.8660254037844387076, 1.000000000000000000, 0.8660254037844387076, 1.000000000000000000, 0.8660254037844387076, 1.000000000000000000, 0.8660254037844387076, 1.000000000000000000, 0.8660254037844387076, 1.000000000000000000, 0.8660254037844387076, 1.000000000000000000, 0.8660254037844387076, 1.000000000000000000, 0.8660254037844387076, 1.000000000000000000, 0.8660254037844387076, 1.000000000000000000, 0.8660254037844387076, 1.000000000000000000, 0.8660254037844387076, 1.000000000000000000, 0.8660254037844387076, 1.000000000000000000, 0.8660254037844387076, 1.000000000000000000, 0.8660254037844387076, 1.000000000000000000, 0.8660254037844387076, 1.000000000000000000, 0.8660254037844387076, 1.000000000000000000, 0.8660254037844387076, 1.000000000000000000, 0.8660254037844387076, 1.000000000000000000, 0.8660254037844387076, 1.000000000000000000, 0.8660254037844387076, 1.000000000000000000, 0.8660254037844387076, 1.000000000000000000, 0.8660254037844387076, 1.000000000000000000, 0.8660254037844387076, 1.000000000000000000, 0.8660254037844387076, 1.000000000000000000, 0.8660254037844387076, 1.000000000000000000, 0.8660254037844387076, 1.000000000000000000, 0.8660254037844387076, 1.000000000000000000, 0.8660254037844387076, 1.000000000000000000, 0.9693186809021840933, 0.9526899265169710418 ) ) 
 REPRESENTATION_ITEM ( '' )  );
#2936 = CARTESIAN_POINT ( 'NONE',  ( -25.11802603177690330, -16.03270077640482683, 0.5379818257722508434 ) ) ;
#2937 = CARTESIAN_POINT ( 'NONE',  ( -25.20430036322041545, -22.07000804769847591, 14.42834449896450799 ) ) ;
#2938 = CARTESIAN_POINT ( 'NONE',  ( 33.23365877489121090, -6.550928303235100891, 5.783357778048664244 ) ) ;
#2939 = AXIS2_PLACEMENT_3D ( 'NONE', #1805, #4920, #2318 ) ;
#2940 = VERTEX_POINT ( 'NONE', #9869 ) ;
#2941 = AXIS2_PLACEMENT_3D ( 'NONE', #3142, #3328, #243 ) ;
#2942 =( NAMED_UNIT ( * ) PLANE_ANGLE_UNIT ( ) SI_UNIT ( $, .RADIAN. ) );
#2943 = ORIENTED_EDGE ( 'NONE', *, *, #12056, .T. ) ;
#2944 = CARTESIAN_POINT ( 'NONE',  ( 26.90793483298705979, -6.248787706170159773, 3.283357778048663356 ) ) ;
#2945 = VERTEX_POINT ( 'NONE', #15424 ) ;
#2946 = DIRECTION ( 'NONE',  ( 1.000000000000000000, -4.440892098500626162E-15, 0.000000000000000000 ) ) ;
#2947 = VECTOR ( 'NONE', #5945, 1000.000000000000114 ) ;
#2948 = CARTESIAN_POINT ( 'NONE',  ( 26.05393439953038381, -7.587479618990243146, -6.529799540429926274 ) ) ;
#2949 = VECTOR ( 'NONE', #10773, 1000.000000000000000 ) ;
#2950 = CARTESIAN_POINT ( 'NONE',  ( 32.55182397003001427, -2.661183353387966299, -3.283357778048662023 ) ) ;
#2951 = CARTESIAN_POINT ( 'NONE',  ( 45.00000000000000711, -16.03270077640482683, 5.537981825772250843 ) ) ;
#2952 = APPLICATION_PROTOCOL_DEFINITION ( 'draft international standard', 'automotive_design', 1998, #2061 ) ;
#2953 = CARTESIAN_POINT ( 'NONE',  ( 33.78529456515154550, -6.484467084455913799, 5.783357778048664244 ) ) ;
#2954 = CARTESIAN_POINT ( 'NONE',  ( 31.66930131758986988, -2.967382423816733894, -3.627061608673662008 ) ) ;
#2955 = LINE ( 'NONE', #8765, #15707 ) ;
#2956 = CARTESIAN_POINT ( 'NONE',  ( 30.52163964716380917, -2.178873678870954400, -4.533357778048659803 ) ) ;
#2957 = AXIS2_PLACEMENT_3D ( 'NONE', #1798, #10206, #9832 ) ;
#2958 = CARTESIAN_POINT ( 'NONE',  ( 30.17635249042624679, -2.520282741259753045, 4.705209693361168455 ) ) ;
#2959 = EDGE_CURVE ( 'NONE', #7076, #5666, #14064, .T. ) ;
#2960 = ORIENTED_EDGE ( 'NONE', *, *, #11162, .F. ) ;
#2961 = CIRCLE ( 'NONE', #15416, 3.000000000000001332 ) ;
#2962 = TOROIDAL_SURFACE ( 'NONE', #13102, 3.199999999999998845, 0.8000000000000001554 ) ;
#2963 =( BOUNDED_CURVE ( )  B_SPLINE_CURVE ( 2, ( #5127, #16219, #13489, #17782, #17866 ),
 .UNSPECIFIED., .F., .T. ) 
 B_SPLINE_CURVE_WITH_KNOTS ( ( 3, 2, 3 ),
 ( 0.000000000000000000, 0.01282051282051282007, 0.01923076923076925265 ),
 .UNSPECIFIED. ) 
 CURVE ( )  GEOMETRIC_REPRESENTATION_ITEM ( )  RATIONAL_B_SPLINE_CURVE ( ( 1.000000000000000000, 0.8660254037844387076, 1.000000000000000000, 0.9330127018922191873, 0.9330127018922194093 ) ) 
 REPRESENTATION_ITEM ( '' )  );
#2964 = ORIENTED_EDGE ( 'NONE', *, *, #16092, .F. ) ;
#2965 = CARTESIAN_POINT ( 'NONE',  ( 28.77978050244509944, -3.315512618508630993, 3.627061608673666893 ) ) ;
#2966 = PRESENTATION_STYLE_ASSIGNMENT (( #9831 ) ) ;
#2967 = CARTESIAN_POINT ( 'NONE',  ( 29.25000000000000000, -16.21813761408365195, -13.00000000000000178 ) ) ;
#2968 = EDGE_CURVE ( 'NONE', #10333, #7372, #1837, .T. ) ;
#2969 = ORIENTED_EDGE ( 'NONE', *, *, #10235, .T. ) ;
#2970 = CARTESIAN_POINT ( 'NONE',  ( 30.74004950963507810, -6.851358974801540214, 5.113484796970852564 ) ) ;
#2971 = EDGE_LOOP ( 'NONE', ( #2037, #12866, #12964, #9958 ) ) ;
#2972 = ORIENTED_EDGE ( 'NONE', *, *, #8391, .T. ) ;
#2973 = CARTESIAN_POINT ( 'NONE',  ( -27.17934203385504333, -30.00000000000000355, 0.000000000000000000 ) ) ;
#2974 = DIRECTION ( 'NONE',  ( -0.1196152422706610735, 0.9928203230275511881, 0.000000000000000000 ) ) ;
#2975 = CYLINDRICAL_SURFACE ( 'NONE', #7300, 13.00000000000000178 ) ;
#2976 = CARTESIAN_POINT ( 'NONE',  ( 26.49878054387835746, -2.963357534503999968, -4.705209693361160461 ) ) ;
#2977 = APPLICATION_CONTEXT ( 'automotive_design' ) ;
#2978 = CARTESIAN_POINT ( 'NONE',  ( 26.59574320524588842, -2.314508053356755024, -5.113484796970857893 ) ) ;
#2979 = CARTESIAN_POINT ( 'NONE',  ( 29.39961944441754227, -3.040961747597316300, -3.283357778048662023 ) ) ;
#2980 =( GEOMETRIC_REPRESENTATION_CONTEXT ( 3 ) GLOBAL_UNCERTAINTY_ASSIGNED_CONTEXT ( ( #14057 ) ) GLOBAL_UNIT_ASSIGNED_CONTEXT ( ( #7945, #5035, #1054 ) ) REPRESENTATION_CONTEXT ( 'NONE', 'WORKASPACE' ) );
#2981 = CARTESIAN_POINT ( 'NONE',  ( 26.12396475346091052, -21.64644127732803014, 14.20549555447399470 ) ) ;
#2982 = CARTESIAN_POINT ( 'NONE',  ( 46.62628598016694070, -0.4028612494373206565, -5.783357778048661579 ) ) ;
#2983 =( NAMED_UNIT ( * ) SI_UNIT ( $, .STERADIAN. ) SOLID_ANGLE_UNIT ( ) );
#2984 = CARTESIAN_POINT ( 'NONE',  ( 32.54050588463559990, -2.235448945602741766, -6.861505862736159145 ) ) ;
#2985 = ORIENTED_EDGE ( 'NONE', *, *, #1916, .F. ) ;
#2986 = FACE_BOUND ( 'NONE', #16908, .T. ) ;
#2987 = DIRECTION ( 'NONE',  ( 1.000000000000000000, 0.000000000000000000, 0.000000000000000000 ) ) ;
#2988 = ADVANCED_FACE ( 'NONE', ( #8616 ), #14148, .T. ) ;
#2989 = ORIENTED_EDGE ( 'NONE', *, *, #3415, .F. ) ;
#2990 = VERTEX_POINT ( 'NONE', #17070 ) ;
#2991 =( GEOMETRIC_REPRESENTATION_CONTEXT ( 3 ) GLOBAL_UNCERTAINTY_ASSIGNED_CONTEXT ( ( #15507 ) ) GLOBAL_UNIT_ASSIGNED_CONTEXT ( ( #16275, #3846, #3749 ) ) REPRESENTATION_CONTEXT ( 'NONE', 'WORKASPACE' ) );
#2992 = ORIENTED_EDGE ( 'NONE', *, *, #3137, .T. ) ;
#2993 = CARTESIAN_POINT ( 'NONE',  ( 28.12741954877813555, -2.767138697495831856, 4.705209693361167567 ) ) ;
#2994 = EDGE_CURVE ( 'NONE', #9531, #3302, #8385, .T. ) ;
#2995 = CARTESIAN_POINT ( 'NONE',  ( 29.34405387406022570, -7.019548880150045633, -5.113484796970862334 ) ) ;
#2996 = CARTESIAN_POINT ( 'NONE',  ( -16.75000000000000000, -16.21813761408365195, -13.00000000000000178 ) ) ;
#2997 = CARTESIAN_POINT ( 'NONE',  ( 32.52441275490655670, -6.636378442139655220, -5.783357778048663356 ) ) ;
#2998 = CARTESIAN_POINT ( 'NONE',  ( 32.96459815279162342, -1.884545423566157174, -4.533357778048659803 ) ) ;
#2999 = CARTESIAN_POINT ( 'NONE',  ( 30.23341599105502908, -5.648260380436597394, -7.939653947423664704 ) ) ;
#3000 = CARTESIAN_POINT ( 'NONE',  ( 11.54660026683835206, 4.788112600790471518, -10.47749643873921244 ) ) ;
#3001 = DIRECTION ( 'NONE',  ( -1.000000000000000000, 0.000000000000000000, 0.000000000000000000 ) ) ;
#3002 = DIRECTION ( 'NONE',  ( 0.000000000000000000, 0.000000000000000000, 1.000000000000000000 ) ) ;
#3003 = EDGE_CURVE ( 'NONE', #1161, #3273, #1203, .T. ) ;
#3004 = UNCERTAINTY_MEASURE_WITH_UNIT (LENGTH_MEASURE( 1.000000000000000082E-05 ), #4939, 'distance_accuracy_value', 'NONE');
#3005 = CARTESIAN_POINT ( 'NONE',  ( 28.55151181693415907, -2.416235175459247486, -4.533357778048659803 ) ) ;
#3006 = CARTESIAN_POINT ( 'NONE',  ( 29.60297508593253468, -5.724216059278466773, -7.939653947423664704 ) ) ;
#3007 = FACE_OUTER_BOUND ( 'NONE', #15954, .T. ) ;
#3008 = CARTESIAN_POINT ( 'NONE',  ( 7.666200962222293747, -6.158133996769738161, -2.333128398347827481 ) ) ;
#3009 = CARTESIAN_POINT ( 'NONE',  ( 26.28374211850152875, -7.120308096563231715, -4.880631602441031447 ) ) ;
#3010 = CARTESIAN_POINT ( 'NONE',  ( 27.92107091181166467, -2.492190854301117753, 7.033357778048666020 ) ) ;
#3011 = EDGE_CURVE ( 'NONE', #15476, #16993, #13400, .T. ) ;
#3012 = CARTESIAN_POINT ( 'NONE',  ( 31.56485473504790917, -1.326280070207274564, 5.783357778048668685 ) ) ;
#3013 = CARTESIAN_POINT ( 'NONE',  ( 28.86293393808771057, -2.678523738846987357, -4.705209693361161349 ) ) ;
#3014 = ORIENTED_EDGE ( 'NONE', *, *, #1141, .F. ) ;
#3015 = ORIENTED_EDGE ( 'NONE', *, *, #13337, .F. ) ;
#3016 = DIRECTION ( 'NONE',  ( 0.9928203230275512992, 0.1196152422706610180, 4.006172263299093133E-17 ) ) ;
#3017 = CARTESIAN_POINT ( 'NONE',  ( 30.40162818048570514, -5.827866652795590241, -3.283357778048667797 ) ) ;
#3018 = ORIENTED_EDGE ( 'NONE', *, *, #1433, .T. ) ;
#3019 = CARTESIAN_POINT ( 'NONE',  ( 0.000000000000000000, 0.000000000000000000, -12.00000000000000000 ) ) ;
#3020 = ORIENTED_EDGE ( 'NONE', *, *, #13579, .F. ) ;
#3021 = CARTESIAN_POINT ( 'NONE',  ( 27.86926259684567597, -5.933094176093607786, -7.939653947423662927 ) ) ;
#3022 = EDGE_CURVE ( 'NONE', #16104, #4963, #12392, .T. ) ;
#3023 = CARTESIAN_POINT ( 'NONE',  ( 28.75786045390062995, -2.691183018653962034, -6.861505862736159145 ) ) ;
#3024 = CARTESIAN_POINT ( 'NONE',  ( 0.000000000000000000, 0.000000000000000000, 8.700000000000001066 ) ) ;
#3025 = CARTESIAN_POINT ( 'NONE',  ( -25.74999999999999289, -16.21813761408365195, 13.00000000000000178 ) ) ;
#3026 = CARTESIAN_POINT ( 'NONE',  ( 31.66250999073069750, -5.675955295111851484, -3.283357778048667797 ) ) ;
#3027 = ADVANCED_FACE ( 'NONE', ( #3958 ), #13572, .T. ) ;
#3028 = CARTESIAN_POINT ( 'NONE',  ( 29.11750682573587312, -2.010685337989277954, -5.113484796970851676 ) ) ;
#3029 = ORIENTED_EDGE ( 'NONE', *, *, #13098, .T. ) ;
#3030 = CARTESIAN_POINT ( 'NONE',  ( 33.30246708102489350, -5.905470865888903020, 6.861505862736158257 ) ) ;
#3031 = ORIENTED_EDGE ( 'NONE', *, *, #11121, .F. ) ;
#3032 = CARTESIAN_POINT ( 'NONE',  ( 26.39370705969127684, -2.976016814310973313, 4.705209693361168455 ) ) ;
#3033 = CARTESIAN_POINT ( 'NONE',  ( -28.92121476417970882, -18.25996810291579209, 13.46562832783231478 ) ) ;
#3034 = CARTESIAN_POINT ( 'NONE',  ( 29.97449477918272009, -6.943593201308171814, 6.453230759126468818 ) ) ;
#3035 = VERTEX_POINT ( 'NONE', #982 ) ;
#3036 = SURFACE_STYLE_FILL_AREA ( #7033 ) ;
#3037 = EDGE_LOOP ( 'NONE', ( #5627, #13441, #17351, #13158 ) ) ;
#3038 = CARTESIAN_POINT ( 'NONE',  ( 33.78529456515154550, -6.484467084455913799, 5.783357778048664244 ) ) ;
#3039 = EDGE_CURVE ( 'NONE', #14228, #15335, #10920, .T. ) ;
#3040 = ORIENTED_EDGE ( 'NONE', *, *, #7175, .T. ) ;
#3041 = CARTESIAN_POINT ( 'NONE',  ( 29.74794773085836397, -1.934729659147405689, -5.113484796970855228 ) ) ;
#3042 = EDGE_CURVE ( 'NONE', #4105, #16322, #12301, .T. ) ;
#3043 = CARTESIAN_POINT ( 'NONE',  ( 26.41562710823574278, -3.600346414165641828, -7.939653947423660263 ) ) ;
#3044 = CARTESIAN_POINT ( 'NONE',  ( 32.97211790677835097, -2.610546234160043610, -8.283357778048658915 ) ) ;
#3045 = CARTESIAN_POINT ( 'NONE',  ( 5.200000000000002842, 0.000000000000000000, 0.000000000000000000 ) ) ;
#3046 =( LENGTH_UNIT ( ) NAMED_UNIT ( * ) SI_UNIT ( .MILLI., .METRE. ) );
#3047 = CARTESIAN_POINT ( 'NONE',  ( 31.23537658942770889, -6.791681843624433945, -5.113484796970860558 ) ) ;
#3048 = CARTESIAN_POINT ( 'NONE',  ( 32.95662993491455950, -6.574107945067995118, -5.783357778048669573 ) ) ;
#3049 = DIRECTION ( 'NONE',  ( 0.000000000000000000, 0.000000000000000000, -1.000000000000000000 ) ) ;
#3050 = LINE ( 'NONE', #11087, #9772 ) ;
#3051 = CARTESIAN_POINT ( 'NONE',  ( 30.78487334700428590, -1.819997462563214263, 5.783357778048668685 ) ) ;
#3052 =( BOUNDED_CURVE ( )  B_SPLINE_CURVE ( 3, ( #7136, #4312, #12648, #4577 ),
 .UNSPECIFIED., .F., .T. ) 
 B_SPLINE_CURVE_WITH_KNOTS ( ( 4, 4 ),
 ( 1.436990331221392081, 1.509167199807614601 ),
 .UNSPECIFIED. ) 
 CURVE ( )  GEOMETRIC_REPRESENTATION_ITEM ( )  RATIONAL_B_SPLINE_CURVE ( ( 1.000000000000000000, 0.9995659220841806025, 0.9995659220841806025, 1.000000000000000000 ) ) 
 REPRESENTATION_ITEM ( '' )  );
#3053 = ORIENTED_EDGE ( 'NONE', *, *, #8958, .T. ) ;
#3054 = ORIENTED_EDGE ( 'NONE', *, *, #278, .F. ) ;
#3055 = CARTESIAN_POINT ( 'NONE',  ( 28.34209327568754233, -5.876127416962207306, 3.627061608673662896 ) ) ;
#3056 = CARTESIAN_POINT ( 'NONE',  ( -31.74999999999995737, 0.000000000000000000, 4.250000000000000000 ) ) ;
#3057 = CARTESIAN_POINT ( 'NONE',  ( 45.00000000000000711, 0.000000000000000000, -5.537981825772250843 ) ) ;
#3058 = ORIENTED_EDGE ( 'NONE', *, *, #17306, .T. ) ;
#3059 = CARTESIAN_POINT ( 'NONE',  ( 30.57046727500519978, -4.353711291323232757, 3.283357778048664244 ) ) ;
#3060 = VERTEX_POINT ( 'NONE', #1249 ) ;
#3061 = CYLINDRICAL_SURFACE ( 'NONE', #4869, 2.500000000000001776 ) ;
#3062 = DIRECTION ( 'NONE',  ( -0.000000000000000000, -0.000000000000000000, -1.000000000000000000 ) ) ;
#3063 = CARTESIAN_POINT ( 'NONE',  ( 2.500000000000000000, 0.000000000000000000, 0.000000000000000000 ) ) ;
#3064 = CARTESIAN_POINT ( 'NONE',  ( 1.243649364574536075E-15, 4.862606272033089816, -3.445885042887437244 ) ) ;
#3065 = CARTESIAN_POINT ( 'NONE',  ( 33.59503905791412137, -1.808589744724287129, -4.533357778048659803 ) ) ;
#3067 = EDGE_CURVE ( 'NONE', #15606, #4693, #9489, .T. ) ;
#3066 = CARTESIAN_POINT ( 'NONE',  ( 32.77257290155422709, -2.834459985843461816, -3.627061608673662896 ) ) ;
#3068 = DIRECTION ( 'NONE',  ( -0.8660254037844397068, -0.4999999999999981126, 0.000000000000000000 ) ) ;
#3069 = CARTESIAN_POINT ( 'NONE',  ( 45.00000000000000711, -19.03270077640483038, 5.537981825772250843 ) ) ;
#3070 = CARTESIAN_POINT ( 'NONE',  ( 31.39792096211754924, -4.254019462947003838, -7.939653947423662039 ) ) ;
#3071 = ORIENTED_EDGE ( 'NONE', *, *, #2857, .F. ) ;
#3072 = EDGE_CURVE ( 'NONE', #9324, #3060, #4044, .T. ) ;
#3073 = CARTESIAN_POINT ( 'NONE',  ( 26.63030083514515312, -6.709335133632020387, -6.861505862736167138 ) ) ;
#3074 = CARTESIAN_POINT ( 'NONE',  ( 3.248936832696173393, -30.00000000000000355, 78.00000000000000000 ) ) ;
#3075 = ORIENTED_EDGE ( 'NONE', *, *, #11293, .F. ) ;
#3076 = ORIENTED_EDGE ( 'NONE', *, *, #8489, .F. ) ;
#3077 = ORIENTED_EDGE ( 'NONE', *, *, #14387, .T. ) ;
#3078 = CARTESIAN_POINT ( 'NONE',  ( 26.86653773853314320, -2.919050055179571945, 4.705209693361167567 ) ) ;
#3079 = ORIENTED_EDGE ( 'NONE', *, *, #6758, .T. ) ;
#3080 = CARTESIAN_POINT ( 'NONE',  ( 28.48706592061337162, -2.086641016831144668, -5.113484796970857893 ) ) ;
#3081 = DIRECTION ( 'NONE',  ( 0.000000000000000000, 0.000000000000000000, -1.000000000000000000 ) ) ;
#3082 = CARTESIAN_POINT ( 'NONE',  ( -7.499998387031003411, -20.49508120620799900, 13.00000000000000178 ) ) ;
#3083 = DIRECTION ( 'NONE',  ( -0.1196152422706610735, 0.9928203230275511881, 0.000000000000000000 ) ) ;
#3084 = CARTESIAN_POINT ( 'NONE',  ( 33.76207435632690590, -3.969185667289998332, -3.627061608673664672 ) ) ;
#3085 = FACE_OUTER_BOUND ( 'NONE', #11150, .T. ) ;
#3086 = FACE_OUTER_BOUND ( 'NONE', #9549, .T. ) ;
#3087 = ORIENTED_EDGE ( 'NONE', *, *, #12395, .F. ) ;
#3088 = EDGE_CURVE ( 'NONE', #7031, #15783, #17355, .T. ) ;
#3089 = CARTESIAN_POINT ( 'NONE',  ( 27.95866967485789090, -6.122194908100387245, -3.283357778048667797 ) ) ;
#3090 = CARTESIAN_POINT ( 'NONE',  ( 26.86291784143654127, -6.981118157082444320, -7.033357778048666908 ) ) ;
#3091 = CARTESIAN_POINT ( 'NONE',  ( 29.51982165028991645, -6.361204938940122844, -4.705209693361168455 ) ) ;
#3092 = FACE_OUTER_BOUND ( 'NONE', #7807, .T. ) ;
#3093 = CARTESIAN_POINT ( 'NONE',  ( 26.31175009776946538, -7.352777558617343168, -6.181997573440047411 ) ) ;
#3094 = ORIENTED_EDGE ( 'NONE', *, *, #738, .T. ) ;
#3095 = ADVANCED_FACE ( 'NONE', ( #14847 ), #5726, .T. ) ;
#3096 = DIRECTION ( 'NONE',  ( 1.000000000000000000, 0.000000000000000000, 0.000000000000000000 ) ) ;
#3097 = CARTESIAN_POINT ( 'NONE',  ( 28.91555989733679866, -4.553094948490599592, 8.283357778048662468 ) ) ;
#3098 = FACE_OUTER_BOUND ( 'NONE', #9375, .T. ) ;
#3099 = EDGE_LOOP ( 'NONE', ( #1086, #10082, #8786, #975 ) ) ;
#3100 = CARTESIAN_POINT ( 'NONE',  ( 26.86291784143654127, -6.981118157082444320, 4.533357778048659803 ) ) ;
#3101 = DIRECTION ( 'NONE',  ( 0.000000000000000000, 0.000000000000000000, 1.000000000000000000 ) ) ;
#3102 = CARTESIAN_POINT ( 'NONE',  ( -23.83446850436624587, -10.01089291621719646, -14.74374009921848483 ) ) ;
#3103 = ORIENTED_EDGE ( 'NONE', *, *, #13488, .T. ) ;
#3104 = AXIS2_PLACEMENT_3D ( 'NONE', #11983, #16358, #17566 ) ;
#3105 = LINE ( 'NONE', #11229, #6131 ) ;
#3106 = CARTESIAN_POINT ( 'NONE',  ( 29.49337484321020497, -2.602568060005117090, -4.705209693361161349 ) ) ;
#3107 = CYLINDRICAL_SURFACE ( 'NONE', #11288, 2.500000000000000444 ) ;
#3108 = DIRECTION ( 'NONE',  ( 0.9928203230275510771, 0.1196152422706609902, 4.006172263299092517E-17 ) ) ;
#3109 = DIRECTION ( 'NONE',  ( -0.000000000000000000, -0.000000000000000000, 1.000000000000000000 ) ) ;
#3110 = EDGE_LOOP ( 'NONE', ( #8128, #11092, #9634 ) ) ;
#3111 = CARTESIAN_POINT ( 'NONE',  ( 32.19529564017040002, -1.250324391365404741, -5.783357778048658027 ) ) ;
#3112 = VERTEX_POINT ( 'NONE', #11936 ) ;
#3113 = CARTESIAN_POINT ( 'NONE',  ( 25.47811240618384687, -2.786519109605914757, 7.033357778048666020 ) ) ;
#3114 = EDGE_CURVE ( 'NONE', #602, #2265, #12023, .T. ) ;
#3115 = AXIS2_PLACEMENT_3D ( 'NONE', #11067, #4205, #14268 ) ;
#3116 = CARTESIAN_POINT ( 'NONE',  ( 28.28955653359400557, -5.882457056865704637, 7.939653947423658487 ) ) ;
#3117 = CARTESIAN_POINT ( 'NONE',  ( -16.91320375285265953, -17.65223671300078223, 16.01217750721622579 ) ) ;
#3118 = CYLINDRICAL_SURFACE ( 'NONE', #12137, 5.000000000000001776 ) ;
#3119 = ORIENTED_EDGE ( 'NONE', *, *, #7617, .T. ) ;
#3120 = DIRECTION ( 'NONE',  ( 0.1196152422706587976, -0.9928203230275515212, 1.866876274697368064E-15 ) ) ;
#3121 = VERTEX_POINT ( 'NONE', #14766 ) ;
#3122 = DIRECTION ( 'NONE',  ( -1.224646799147353207E-16, 1.000000000000000000, 0.000000000000000000 ) ) ;
#3123 = EDGE_CURVE ( 'NONE', #14839, #8562, #15222, .T. ) ;
#3124 = ORIENTED_EDGE ( 'NONE', *, *, #16637, .T. ) ;
#3125 = CARTESIAN_POINT ( 'NONE',  ( 30.54048978798443059, -6.538043363838207611, -4.533357778048668685 ) ) ;
#3126 = CARTESIAN_POINT ( 'NONE',  ( 28.49970350196817392, -5.857138497251738407, -7.939653947423664704 ) ) ;
#3127 = CARTESIAN_POINT ( 'NONE',  ( 31.08079519141086777, -2.838413270685653078, -8.283357778048658915 ) ) ;
#3128 = CARTESIAN_POINT ( 'NONE',  ( 26.01652455409633902, -4.902371455920926380, 5.783357778048663356 ) ) ;
#3129 = FACE_BOUND ( 'NONE', #12977, .T. ) ;
#3130 = CARTESIAN_POINT ( 'NONE',  ( 29.55043834383899437, -5.730545699181964991, -3.627061608673668225 ) ) ;
#3131 = CARTESIAN_POINT ( 'NONE',  ( 32.19919549706052209, -6.038393303862174655, -4.705209693361169343 ) ) ;
#3132 = CIRCLE ( 'NONE', #6317, 2.749999999999988454 ) ;
#3133 = DIRECTION ( 'NONE',  ( 0.000000000000000000, 0.000000000000000000, 1.000000000000000000 ) ) ;
#3135 = AXIS2_PLACEMENT_3D ( 'NONE', #16840, #16558, #7048 ) ;
#3134 = CARTESIAN_POINT ( 'NONE',  ( 3.199999999999998845, 0.000000000000000000, 1.599999999999999423 ) ) ;
#3136 = CARTESIAN_POINT ( 'NONE',  ( 30.82871344409320713, -3.068656662272551738, 3.627061608673666893 ) ) ;
#3137 = EDGE_CURVE ( 'NONE', #3302, #6631, #2380, .T. ) ;
#3138 = ORIENTED_EDGE ( 'NONE', *, *, #5131, .F. ) ;
#3139 = CARTESIAN_POINT ( 'NONE',  ( 26.24651417059167002, -6.811311830135040601, 7.170103614070669096 ) ) ;
#3140 = ORIENTED_EDGE ( 'NONE', *, *, #16607, .F. ) ;
#3141 = CARTESIAN_POINT ( 'NONE',  ( 30.25533603959949502, -6.272589980291270351, 4.705209693361160461 ) ) ;
#3142 = CARTESIAN_POINT ( 'NONE',  ( 5.384454397937117776, 0.000000000000000000, -4.184454397937119374 ) ) ;
#3143 = CARTESIAN_POINT ( 'NONE',  ( 15.92260893619738837, -28.39189527176317540, 0.000000000000000000 ) ) ;
#3144 = ORIENTED_EDGE ( 'NONE', *, *, #10769, .F. ) ;
#3145 = CARTESIAN_POINT ( 'NONE',  ( 27.67650891848073158, -3.448435056481901295, 3.627061608673666449 ) ) ;
#3146 = CIRCLE ( 'NONE', #3729, 2.001963570546864801 ) ;
#3147 = CARTESIAN_POINT ( 'NONE',  ( 27.53837573810955419, -6.172832027328289506, 3.283357778048663356 ) ) ;
#3148 = DIRECTION ( 'NONE',  ( -1.000000000000000000, -0.000000000000000000, -0.000000000000000000 ) ) ;
#3149 = CARTESIAN_POINT ( 'NONE',  ( -35.77680296528374271, -19.03270077640483038, 0.5379818257722512875 ) ) ;
#3150 = CARTESIAN_POINT ( 'NONE',  ( 25.61697401368257587, -3.496695820648536568, -3.283357778048662023 ) ) ;
#3151 = CARTESIAN_POINT ( 'NONE',  ( 33.40745134805642635, -4.011910736534825439, -3.283357778048664688 ) ) ;
#3152 = CARTESIAN_POINT ( 'NONE',  ( -20.00000000000000000, 7.999999999999996447, -15.51150668642334374 ) ) ;
#3153 =( NAMED_UNIT ( * ) PLANE_ANGLE_UNIT ( ) SI_UNIT ( $, .RADIAN. ) );
#3154 = CARTESIAN_POINT ( 'NONE',  ( 30.75425665345519732, -2.450656702321377001, -4.705209693361161349 ) ) ;
#3155 = CARTESIAN_POINT ( 'NONE',  ( 26.39823381822652593, -6.110324093391315436, -3.627061608673668225 ) ) ;
#3156 = CARTESIAN_POINT ( 'NONE',  ( -37.55714628004649569, -12.56174331051002113, 5.783357778048663356 ) ) ;
#3157 = EDGE_CURVE ( 'NONE', #8806, #13014, #9501, .T. ) ;
#3158 = ORIENTED_EDGE ( 'NONE', *, *, #9234, .T. ) ;
#3159 = EDGE_LOOP ( 'NONE', ( #16768, #15799, #16584 ) ) ;
#3160 = ORIENTED_EDGE ( 'NONE', *, *, #10235, .F. ) ;
#3161 = CARTESIAN_POINT ( 'NONE',  ( 28.13194630731337753, -5.901445976576172647, 7.939653947423658487 ) ) ;
#3162 = DIRECTION ( 'NONE',  ( 0.1113444980252557837, -0.9937818688019538493, 0.000000000000000000 ) ) ;
#3163 = FACE_OUTER_BOUND ( 'NONE', #13989, .T. ) ;
#3164 = CARTESIAN_POINT ( 'NONE',  ( 5.384454397937117776, 0.000000000000000000, -4.700000000000000178 ) ) ;
#3165 = CARTESIAN_POINT ( 'NONE',  ( 20.00000000000000355, 7.999999999999996447, -6.000000000000000000 ) ) ;
#3166 = CARTESIAN_POINT ( 'NONE',  ( 31.66930131758986988, -2.967382423816733894, -3.627061608673662008 ) ) ;
#3167 = CARTESIAN_POINT ( 'NONE',  ( -3.680118525130244400, 2.494084732383329062, -0.3507732604232482454 ) ) ;
#3168 = EDGE_CURVE ( 'NONE', #15953, #8806, #4403, .T. ) ;
#3169 = CARTESIAN_POINT ( 'NONE',  ( 45.00000000000000711, -16.03270077640482683, -10.53798182577225084 ) ) ;
#3170 = VECTOR ( 'NONE', #16599, 1000.000000000000227 ) ;
#3171 = DIRECTION ( 'NONE',  ( -1.000000000000000000, 0.000000000000000000, 0.000000000000000000 ) ) ;
#3172 = FACE_OUTER_BOUND ( 'NONE', #10594, .T. ) ;
#3173 = ORIENTED_EDGE ( 'NONE', *, *, #1569, .F. ) ;
#3174 = CARTESIAN_POINT ( 'NONE',  ( 31.91459173804834748, -5.445711903524953712, -3.627061608673667781 ) ) ;
#3175 = DIRECTION ( 'NONE',  ( 0.000000000000000000, 0.000000000000000000, -1.000000000000000000 ) ) ;
#3176 = CARTESIAN_POINT ( 'NONE',  ( 32.55182397003001427, -2.661183353387966299, -3.283357778048662023 ) ) ;
#3177 = CARTESIAN_POINT ( 'NONE',  ( 26.31376129264122810, -7.369470708288995198, -5.989870097397514748 ) ) ;
#3178 = VECTOR ( 'NONE', #4550, 1000.000000000000227 ) ;
#3179 = LINE ( 'NONE', #15329, #5442 ) ;
#3180 = CARTESIAN_POINT ( 'NONE',  ( 29.35089333861488115, -5.954459450865362768, 3.283357778048663800 ) ) ;
#3181 = CARTESIAN_POINT ( 'NONE',  ( -23.00000000000000000, -16.21813761408365195, -13.00000000000000178 ) ) ;
#3182 = VECTOR ( 'NONE', #1774, 1000.000000000000114 ) ;
#3183 = EDGE_CURVE ( 'NONE', #9522, #1377, #13265, .T. ) ;
#3184 = ORIENTED_EDGE ( 'NONE', *, *, #17716, .F. ) ;
#3185 = ORIENTED_EDGE ( 'NONE', *, *, #4228, .F. ) ;
#3186 = CARTESIAN_POINT ( 'NONE',  ( 26.31556265977298992, -7.384422263489805793, 5.783357778048663356 ) ) ;
#3187 = ORIENTED_EDGE ( 'NONE', *, *, #3576, .T. ) ;
#3188 = ORIENTED_EDGE ( 'NONE', *, *, #14174, .F. ) ;
#3189 = CARTESIAN_POINT ( 'NONE',  ( -17.31608032955932330, -13.61075944537037508, -15.95276485144012035 ) ) ;
#3190 = EDGE_LOOP ( 'NONE', ( #4795, #17103, #11231, #9291, #13094, #3504 ) ) ;
#3191 = CIRCLE ( 'NONE', #1754, 5.000000000000000000 ) ;
#3192 = EDGE_CURVE ( 'NONE', #14557, #9400, #4492, .T. ) ;
#3193 = LINE ( 'NONE', #8730, #11627 ) ;
#3194 = CARTESIAN_POINT ( 'NONE',  ( 26.58890374069123652, -3.379597482641427231, -8.283357778048660691 ) ) ;
#3195 = CARTESIAN_POINT ( 'NONE',  ( 29.41022140756759029, -3.239556939666760726, -7.939653947423660263 ) ) ;
#3196 = CARTESIAN_POINT ( 'NONE',  ( 28.11132641904908169, -7.168068194032743534, -5.783357778048668685 ) ) ;
#3197 = CARTESIAN_POINT ( 'NONE',  ( 33.16732689266149237, -6.221561368663743430, -7.033357778048666908 ) ) ;
#3198 = FACE_OUTER_BOUND ( 'NONE', #15405, .T. ) ;
#3199 = CARTESIAN_POINT ( 'NONE',  ( 32.43181250335191379, -6.310176327312596811, -4.533357778048668685 ) ) ;
#3200 = CARTESIAN_POINT ( 'NONE',  ( 29.07687923786957285, -2.352938776424351008, -7.033357778048658027 ) ) ;
#3201 = ORIENTED_EDGE ( 'NONE', *, *, #1899, .F. ) ;
#3202 = CARTESIAN_POINT ( 'NONE',  ( 26.06734695949040059, -6.350061944625998933, 8.283357778048658915 ) ) ;
#3203 = AXIS2_PLACEMENT_3D ( 'NONE', #13059, #12881, #8529 ) ;
#3204 = EDGE_CURVE ( 'NONE', #1502, #3497, #6750, .T. ) ;
#3205 = AXIS2_PLACEMENT_3D ( 'NONE', #10231, #10312, #10043 ) ;
#3206 = CARTESIAN_POINT ( 'NONE',  ( 31.34233605952372415, -6.778795339760710803, 5.783357778048664244 ) ) ;
#3207 = CARTESIAN_POINT ( 'NONE',  ( -28.29220412912503946, -19.54937045720491184, 13.63977809545137454 ) ) ;
#3208 = LINE ( 'NONE', #6002, #13005 ) ;
#3209 = ADVANCED_FACE ( 'NONE', ( #8299 ), #16934, .T. ) ;
#3210 = ORIENTED_EDGE ( 'NONE', *, *, #6008, .T. ) ;
#3211 = CARTESIAN_POINT ( 'NONE',  ( -5.237433445017501299, -16.51494876461869765, 16.99438405180048761 ) ) ;
#3212 = EDGE_LOOP ( 'NONE', ( #1873, #392, #4874, #1589, #10059 ) ) ;
#3213 = DIRECTION ( 'NONE',  ( 0.000000000000000000, 0.000000000000000000, 1.000000000000000000 ) ) ;
#3214 = LINE ( 'NONE', #16670, #6412 ) ;
#3215 = EDGE_LOOP ( 'NONE', ( #9786, #351 ) ) ;
#3216 = CARTESIAN_POINT ( 'NONE',  ( 29.95125523467787332, -2.974500528818129652, -3.283357778048662023 ) ) ;
#3217 = EDGE_CURVE ( 'NONE', #11718, #7736, #3050, .T. ) ;
#3218 = CARTESIAN_POINT ( 'NONE',  ( 32.46178999037268653, -4.125844254797621957, -8.283357778048662468 ) ) ;
#3219 = CARTESIAN_POINT ( 'NONE',  ( 41.90164972253718645, -2.988527579590353422, -5.783357778048662468 ) ) ;
#3220 = SHAPE_DEFINITION_REPRESENTATION ( #17387, #12598 ) ;
#3221 = FACE_BOUND ( 'NONE', #16571, .T. ) ;
#3222 = CARTESIAN_POINT ( 'NONE',  ( 33.23365877489121090, -6.550928303235100891, -5.783357778048663356 ) ) ;
#3223 = AXIS2_PLACEMENT_3D ( 'NONE', #9509, #15053, #6709 ) ;
#3224 = CARTESIAN_POINT ( 'NONE',  ( 26.85044460880409645, -7.319979551716484067, -5.783357778048668685 ) ) ;
#3225 = CARTESIAN_POINT ( 'NONE',  ( 31.21213704492286212, -2.822589171134389563, -3.283357778048662023 ) ) ;
#3226 = CARTESIAN_POINT ( 'NONE',  ( 28.51709679197739078, -3.347160818026084339, 7.939653947423664704 ) ) ;
#3227 = SHAPE_REPRESENTATION ( 'BR-592', ( #11703, #8847, #1031, #1620, #17274, #11127, #5638, #14061, #10563, #7983, #6240, #13196, #2211, #4504, #9382, #3899, #12573, #4751, #14895 ), #17244 ) ;
#3228 = EDGE_CURVE ( 'NONE', #9477, #16479, #8486, .T. ) ;
#3229 = VECTOR ( 'NONE', #17641, 999.9999999999998863 ) ;
#3230 = VERTEX_POINT ( 'NONE', #15279 ) ;
#3231 = STYLED_ITEM ( 'NONE', ( #2966 ), #11368 ) ;
#3232 = CARTESIAN_POINT ( 'NONE',  ( 25.97837335112617652, -4.585712065882579402, 7.940391451607452744 ) ) ;
#3233 = ORIENTED_EDGE ( 'NONE', *, *, #17773, .F. ) ;
#3234 = CARTESIAN_POINT ( 'NONE',  ( 32.28234893270314387, -5.401404424200516807, 3.627061608673662896 ) ) ;
#3235 = CARTESIAN_POINT ( 'NONE',  ( 26.01652455409633902, -4.902371455920926380, 5.783357778048663356 ) ) ;
#3236 = CARTESIAN_POINT ( 'NONE',  ( 26.31128205117621022, -7.047579375861630524, -7.033357778048666908 ) ) ;
#3237 = EDGE_LOOP ( 'NONE', ( #17265, #5595, #321, #9664 ) ) ;
#3238 = AXIS2_PLACEMENT_3D ( 'NONE', #17315, #6409, #9130 ) ;
#3239 =( LENGTH_UNIT ( ) NAMED_UNIT ( * ) SI_UNIT ( .MILLI., .METRE. ) );
#3240 = VECTOR ( 'NONE', #6438, 1000.000000000000000 ) ;
#3241 = CARTESIAN_POINT ( 'NONE',  ( 35.41536221060850664, -16.03270077640482683, -10.53798182577225084 ) ) ;
#3242 = DIRECTION ( 'NONE',  ( -1.000000000000000000, -0.000000000000000000, -0.000000000000000000 ) ) ;
#3243 = CARTESIAN_POINT ( 'NONE',  ( 4.000000000000000000, -6.071532165918824830E-15, -2.842992957459234749 ) ) ;
#3244 = CARTESIAN_POINT ( 'NONE',  ( 25.33925079868512498, -2.076342398563292058, -5.783357778048658027 ) ) ;
#3245 = EDGE_CURVE ( 'NONE', #8066, #12145, #6895, .T. ) ;
#3246 = DIRECTION ( 'NONE',  ( 0.000000000000000000, 0.000000000000000000, -1.000000000000000000 ) ) ;
#3247 = CIRCLE ( 'NONE', #2096, 2.749999999999988454 ) ;
#3248 = DIRECTION ( 'NONE',  ( 1.000000000000000000, 0.000000000000000000, 0.000000000000000000 ) ) ;
#3249 = CARTESIAN_POINT ( 'NONE',  ( 30.01874226414561875, -2.539271660970221944, -6.861505862736159145 ) ) ;
#3250 = ORIENTED_EDGE ( 'NONE', *, *, #1159, .F. ) ;
#3251 = DIRECTION ( 'NONE',  ( 0.9928203230275510771, 0.1196152422706621282, -0.000000000000000000 ) ) ;
#3252 = CARTESIAN_POINT ( 'NONE',  ( 32.97211790677835097, -2.610546234160043610, 3.283357778048666464 ) ) ;
#3253 = TOROIDAL_SURFACE ( 'NONE', #12514, 12.70000000000000284, 0.9000000000000003553 ) ;
#3254 = EDGE_CURVE ( 'NONE', #8113, #2945, #9214, .T. ) ;
#3255 = ORIENTED_EDGE ( 'NONE', *, *, #12421, .T. ) ;
#3256 = ORIENTED_EDGE ( 'NONE', *, *, #16158, .T. ) ;
#3257 = EDGE_LOOP ( 'NONE', ( #17364, #11314 ) ) ;
#3258 = CARTESIAN_POINT ( 'NONE',  ( 28.38593337277646711, -7.124786616671554107, 5.783357778048658915 ) ) ;
#3259 = AXIS2_PLACEMENT_3D ( 'NONE', #5486, #6945, #15287 ) ;
#3260 = CARTESIAN_POINT ( 'NONE',  ( 33.32855701603872234, -2.140504347050403045, 4.705209693361168455 ) ) ;
#3261 = DIRECTION ( 'NONE',  ( -0.1196152422706611984, 0.9928203230275510771, 0.000000000000000000 ) ) ;
#3262 = LINE ( 'NONE', #15682, #1156 ) ;
#3263 = CIRCLE ( 'NONE', #13399, 2.000000000000001776 ) ;
#3264 = CARTESIAN_POINT ( 'NONE',  ( -29.20851401586840979, -17.04915871481012246, -13.38439546398730329 ) ) ;
#3265 = CARTESIAN_POINT ( 'NONE',  ( 32.93470988637010066, -5.949778345213319497, -6.861505862736167138 ) ) ;
#3266 = CARTESIAN_POINT ( 'NONE',  ( -3.355112389629168579, 2.681727112203154295, -0.2256878752776713681 ) ) ;
#3267 = DIRECTION ( 'NONE',  ( 0.1196152422706597829, -0.9928203230275514102, 0.000000000000000000 ) ) ;
#3268 = CIRCLE ( 'NONE', #17489, 1.000000000000000000 ) ;
#3269 = AXIS2_PLACEMENT_3D ( 'NONE', #1979, #6133, #442 ) ;
#3270 = CARTESIAN_POINT ( 'NONE',  ( 29.45101334415624095, -7.006662376286321603, -5.783357778048657138 ) ) ;
#3271 = CARTESIAN_POINT ( 'NONE',  ( 1.317756351988340180, -3.857995168970211441, -0.04852650426602252154 ) ) ;
#3272 = CARTESIAN_POINT ( 'NONE',  ( 26.89670596474818609, -7.703954147932045693, -5.783357778048669573 ) ) ;
#3273 = VERTEX_POINT ( 'NONE', #1514 ) ;
#3274 = VERTEX_POINT ( 'NONE', #4227 ) ;
#3275 = CARTESIAN_POINT ( 'NONE',  ( 26.98483462626008134, -4.785709214840094816, -7.939653947423662039 ) ) ;
#3276 = CARTESIAN_POINT ( 'NONE',  ( -45.00000000000000711, -19.03270077640483038, -5.537981825772250843 ) ) ;
#3277 = CARTESIAN_POINT ( 'NONE',  ( 32.69820532807177216, -4.097360875439379768, -3.283357778048664688 ) ) ;
#3278 = CARTESIAN_POINT ( 'NONE',  ( -4.281152949374479100, 4.203775615332271620, -2.000000000000000000 ) ) ;
#3279 = CARTESIAN_POINT ( 'NONE',  ( 3.680118525130243512, -2.494084732383340608, -0.3507732604232518536 ) ) ;
#3280 = VECTOR ( 'NONE', #6407, 1000.000000000000000 ) ;
#3281 = CARTESIAN_POINT ( 'NONE',  ( 29.70732014299206369, -2.276983097582480742, 4.533357778048667797 ) ) ;
#3282 = CYLINDRICAL_SURFACE ( 'NONE', #17636, 2.500000000000001776 ) ;
#3283 = AXIS2_PLACEMENT_3D ( 'NONE', #5830, #4482, #14012 ) ;
#3284 = ORIENTED_EDGE ( 'NONE', *, *, #10028, .F. ) ;
#3285 = FACE_OUTER_BOUND ( 'NONE', #8751, .T. ) ;
#3286 = ORIENTED_EDGE ( 'NONE', *, *, #1913, .F. ) ;
#3287 = DIRECTION ( 'NONE',  ( 0.000000000000000000, -1.000000000000000000, -3.469446951953614189E-16 ) ) ;
#3288 = VECTOR ( 'NONE', #15873, 1000.000000000000227 ) ;
#3289 = DIRECTION ( 'NONE',  ( 1.000000000000000000, 0.000000000000000000, 0.000000000000000000 ) ) ;
#3290 = CARTESIAN_POINT ( 'NONE',  ( 25.99533317148741318, -3.650983533393564517, -3.627061608673662008 ) ) ;
#3291 = CARTESIAN_POINT ( 'NONE',  ( 25.99533317148741318, -3.650983533393564517, -3.627061608673662008 ) ) ;
#3292 = EDGE_CURVE ( 'NONE', #11171, #14411, #8219, .T. ) ;
#3293 = CARTESIAN_POINT ( 'NONE',  ( 28.10549950023366961, -2.142809097641162897, -5.783357778048658027 ) ) ;
#3294 = ORIENTED_EDGE ( 'NONE', *, *, #11753, .F. ) ;
#3295 = CARTESIAN_POINT ( 'NONE',  ( 26.01652455409633902, -4.902371455920928156, -5.783357778048663356 ) ) ;
#3296 = CARTESIAN_POINT ( 'NONE',  ( 33.48996557372703364, -1.821249024531260696, -7.033357778048658027 ) ) ;
#3297 = ORIENTED_EDGE ( 'NONE', *, *, #7038, .F. ) ;
#3298 = CARTESIAN_POINT ( 'NONE',  ( 29.95125523467787687, -2.974500528818130096, -3.283357778048662023 ) ) ;
#3299 = CARTESIAN_POINT ( 'NONE',  ( 39.19942832275109623, -5.640193629429878897, -9.783357778048662468 ) ) ;
#3300 = EDGE_CURVE ( 'NONE', #14246, #13718, #3052, .T. ) ;
#3301 = CARTESIAN_POINT ( 'NONE',  ( 26.31128205117621022, -7.047579375861630524, 4.533357778048659803 ) ) ;
#3302 = VERTEX_POINT ( 'NONE', #12563 ) ;
#3303 = CARTESIAN_POINT ( 'NONE',  ( 30.74004950963507810, -6.851358974801540214, -6.453230759126470595 ) ) ;
#3304 = DIRECTION ( 'NONE',  ( 1.000000000000000000, 0.000000000000000000, 0.000000000000000000 ) ) ;
#3305 = ORIENTED_EDGE ( 'NONE', *, *, #8060, .T. ) ;
#3306 = DIRECTION ( 'NONE',  ( 0.000000000000000000, 0.000000000000000000, -1.000000000000000000 ) ) ;
#3307 = VERTEX_POINT ( 'NONE', #15920 ) ;
#3308 = LINE ( 'NONE', #134, #6075 ) ;
#3309 = DIRECTION ( 'NONE',  ( -0.000000000000000000, -0.000000000000000000, -1.000000000000000000 ) ) ;
#3310 = CARTESIAN_POINT ( 'NONE',  ( 27.32822876973539294, -6.198150586942257512, -3.283357778048667797 ) ) ;
#3311 = ADVANCED_FACE ( 'NONE', ( #774 ), #6021, .T. ) ;
#3312 = AXIS2_PLACEMENT_3D ( 'NONE', #5444, #12434, #16617 ) ;
#3313 = DIRECTION ( 'NONE',  ( 0.9928203230275512992, 0.1196152422706610180, 4.006172263299093133E-17 ) ) ;
#3314 = DIRECTION ( 'NONE',  ( 0.000000000000000000, 0.000000000000000000, -1.000000000000000000 ) ) ;
#3315 = ITEM_DEFINED_TRANSFORMATION ( 'NONE', 'NONE', #11127,  #3575 ) ;
#3316 = FACE_OUTER_BOUND ( 'NONE', #5844, .T. ) ;
#3317 =( BOUNDED_CURVE ( )  B_SPLINE_CURVE ( 3, ( #2473, #15996, #10606, #13352 ),
 .UNSPECIFIED., .F., .T. ) 
 B_SPLINE_CURVE_WITH_KNOTS ( ( 4, 4 ),
 ( 4.363323129985829496, 4.457746946181837977 ),
 .UNSPECIFIED. ) 
 CURVE ( )  GEOMETRIC_REPRESENTATION_ITEM ( )  RATIONAL_B_SPLINE_CURVE ( ( 1.000000000000000000, 0.9992571499088201969, 0.9992571499088201969, 1.000000000000000000 ) ) 
 REPRESENTATION_ITEM ( '' )  );
#3318 = CARTESIAN_POINT ( 'NONE',  ( 32.04575515724926760, -1.668086104879473730, -5.783357778048658027 ) ) ;
#3319 = CARTESIAN_POINT ( 'NONE',  ( -7.958171371211089529, -6.326703190994665604, -2.666481567098319516 ) ) ;
#3320 = CARTESIAN_POINT ( 'NONE',  ( 33.73390066541284682, -2.518766455766909385, 8.283357778048664244 ) ) ;
#3321 = ORIENTED_EDGE ( 'NONE', *, *, #7868, .F. ) ;
#3322 = EDGE_CURVE ( 'NONE', #9702, #14428, #1965, .T. ) ;
#3323 =( BOUNDED_CURVE ( )  B_SPLINE_CURVE ( 2, ( #16602, #8252, #1193, #13785, #6888, #15147, #9340, #8333, #16428 ),
 .UNSPECIFIED., .F., .T. ) 
 B_SPLINE_CURVE_WITH_KNOTS ( ( 3, 2, 2, 2, 3 ),
 ( 0.09615384615384617306, 0.1025641025641025605, 0.1153846153846153910, 0.1282051282051281937, 0.1346153846153846367 ),
 .UNSPECIFIED. ) 
 CURVE ( )  GEOMETRIC_REPRESENTATION_ITEM ( )  RATIONAL_B_SPLINE_CURVE ( ( 0.9330127018922194093, 0.9330127018922196314, 1.000000000000000000, 0.8660254037844387076, 1.000000000000000000, 0.8660254037844387076, 1.000000000000000000, 0.9330127018922190762, 0.9330127018922194093 ) ) 
 REPRESENTATION_ITEM ( '' )  );
#3324 = ORIENTED_EDGE ( 'NONE', *, *, #9142, .F. ) ;
#3325 = CARTESIAN_POINT ( 'NONE',  ( 25.93714794488954212, -2.393855775999666591, -5.783357778048658027 ) ) ;
#3326 = ORIENTED_EDGE ( 'NONE', *, *, #13518, .T. ) ;
#3327 = CARTESIAN_POINT ( 'NONE',  ( 32.04575515724926760, -1.668086104879473730, 5.783357778048668685 ) ) ;
#3328 = DIRECTION ( 'NONE',  ( 0.000000000000000000, -1.000000000000000000, 0.000000000000000000 ) ) ;
#3329 = CARTESIAN_POINT ( 'NONE',  ( 42.32364987186199556, -2.937684895442014277, -5.783357778048662468 ) ) ;
#3330 = ORIENTED_EDGE ( 'NONE', *, *, #6121, .T. ) ;
#3331 = DIRECTION ( 'NONE',  ( -0.000000000000000000, -0.000000000000000000, 1.000000000000000000 ) ) ;
#3332 = CARTESIAN_POINT ( 'NONE',  ( 27.41826274939272423, -4.733489685532582314, 3.283357778048664244 ) ) ;
#3333 = CARTESIAN_POINT ( 'NONE',  ( 5.499998817156067865, -20.49639288455253450, -6.000000000000000000 ) ) ;
#3334 = CARTESIAN_POINT ( 'NONE',  ( 33.58707084003705745, -6.498152266226123963, -5.783357778048669573 ) ) ;
#3335 = CARTESIAN_POINT ( 'NONE',  ( 26.27749392786457250, -6.324743385012029151, -8.283357778048662468 ) ) ;
#3336 = CARTESIAN_POINT ( 'NONE',  ( 28.40369292566375492, -19.36532336263649512, 13.60921607110385523 ) ) ;
#3337 = CARTESIAN_POINT ( 'NONE',  ( 45.00000000000000711, 0.000000000000000000, 5.537981825772250843 ) ) ;
#3338 = CARTESIAN_POINT ( 'NONE',  ( 28.88938074516742205, -6.437160617781993999, -4.705209693361168455 ) ) ;
#3339 = SHAPE_REPRESENTATION ( 'socket head cap screw_iso_ISO 4762 M5 x 35 - 22N', ( #3575 ), #5366 ) ;
#3340 = CARTESIAN_POINT ( 'NONE',  ( 27.23882169172318513, -6.009049854935478052, -7.939653947423662927 ) ) ;
#3341 = CARTESIAN_POINT ( 'NONE',  ( 30.57046727500519978, -4.353711291323232757, 3.283357778048664244 ) ) ;
#3342 = VERTEX_POINT ( 'NONE', #6301 ) ;
#3343 = ORIENTED_EDGE ( 'NONE', *, *, #3467, .T. ) ;
#3344 = ORIENTED_EDGE ( 'NONE', *, *, #5310, .T. ) ;
#3345 = EDGE_CURVE ( 'NONE', #13298, #4903, #1397, .T. ) ;
#3346 = FACE_OUTER_BOUND ( 'NONE', #5790, .T. ) ;
#3347 = DIRECTION ( 'NONE',  ( -1.000000000000000000, 0.000000000000000000, 0.000000000000000000 ) ) ;
#3348 = CARTESIAN_POINT ( 'NONE',  ( 46.62628598016694781, -0.4028612494373219333, -5.783357778048661579 ) ) ;
#3349 = CARTESIAN_POINT ( 'NONE',  ( 11.54660026683835206, 4.788112600790471518, -8.722503561260788629 ) ) ;
#3350 = PLANE ( 'NONE',  #5811 ) ;
#3351 = CARTESIAN_POINT ( 'NONE',  ( 33.44685390376565692, -4.007163506710925027, -7.939653947423662039 ) ) ;
#3352 = CARTESIAN_POINT ( 'NONE',  ( 30.61177514885986639, -5.802548093181622235, -8.283357778048664244 ) ) ;
#3353 = CARTESIAN_POINT ( 'NONE',  ( -21.42601376483257880, 2.765314980223223529, 6.000000000000000000 ) ) ;
#3354 = VERTEX_POINT ( 'NONE', #2154 ) ;
#3355 = CARTESIAN_POINT ( 'NONE',  ( 28.76917853929504432, -3.116917426439186123, -3.283357778048662023 ) ) ;
#3356 = CARTESIAN_POINT ( 'NONE',  ( 39.99999999999999289, 0.000000000000000000, 0.000000000000000000 ) ) ;
#3357 = EDGE_CURVE ( 'NONE', #1615, #14070, #251, .T. ) ;
#3358 = CARTESIAN_POINT ( 'NONE',  ( 8.472608240843633681E-22, -7.722472891792491889E-22, -7.794427190999915211 ) ) ;
#3359 = ORIENTED_EDGE ( 'NONE', *, *, #11795, .F. ) ;
#3360 = VERTEX_POINT ( 'NONE', #6213 ) ;
#3361 = CARTESIAN_POINT ( 'NONE',  ( 25.81100034576892455, -6.186289477007987259, -7.540293452860097112 ) ) ;
#3362 = FACE_OUTER_BOUND ( 'NONE', #5487, .T. ) ;
#3363 = ORIENTED_EDGE ( 'NONE', *, *, #12537, .T. ) ;
#3364 = CARTESIAN_POINT ( 'NONE',  ( 27.17934203385504333, -30.00000000000000355, -12.00000000000000000 ) ) ;
#3365 = CARTESIAN_POINT ( 'NONE',  ( 27.65467808709180630, -4.705006306174339237, 8.283357778048662468 ) ) ;
#3366 = VERTEX_POINT ( 'NONE', #427 ) ;
#3367 = ADVANCED_FACE ( 'NONE', ( #11823 ), #11513, .F. ) ;
#3368 = FACE_BOUND ( 'NONE', #15608, .T. ) ;
#3369 = EDGE_CURVE ( 'NONE', #15678, #5342, #7488, .T. ) ;
#3370 = CARTESIAN_POINT ( 'NONE',  ( 31.25770402584614871, -1.763030703431812451, -5.783357778048658915 ) ) ;
#3371 = ORIENTED_EDGE ( 'NONE', *, *, #2209, .T. ) ;
#3372 = DIRECTION ( 'NONE',  ( -0.1196152422706609625, 0.9928203230275510771, 0.000000000000000000 ) ) ;
#3373 = CARTESIAN_POINT ( 'NONE',  ( -35.74085044863416272, -18.73429073671335132, -11.27079897466147607 ) ) ;
#3374 = CARTESIAN_POINT ( 'NONE',  ( 27.91310269393460430, -7.181753375802955475, -5.783357778048669573 ) ) ;
#3375 = ORIENTED_EDGE ( 'NONE', *, *, #4866, .T. ) ;
#3376 = DIRECTION ( 'NONE',  ( 0.9928203230275510771, 0.1196152422706609902, 4.006172263299092517E-17 ) ) ;
#3377 = CARTESIAN_POINT ( 'NONE',  ( 25.58373587974369201, -2.446631813008643075, -5.783357778048658027 ) ) ;
#3378 = DIRECTION ( 'NONE',  ( -0.000000000000000000, -0.000000000000000000, 1.000000000000000000 ) ) ;
#3379 = CARTESIAN_POINT ( 'NONE',  ( 33.50243880635947846, -1.482387629897225390, -5.783357778048663356 ) ) ;
#3380 = DIRECTION ( 'NONE',  ( 0.000000000000000000, 0.000000000000000000, -1.000000000000000000 ) ) ;
#3381 = CARTESIAN_POINT ( 'NONE',  ( 29.35089333861488115, -5.954459450865362768, -8.283357778048662468 ) ) ;
#3382 = CARTESIAN_POINT ( 'NONE',  ( -10.89999065189540772, -4.519978295146205305, -9.600000000000001421 ) ) ;
#3383 = CARTESIAN_POINT ( 'NONE',  ( 31.53813789838894621, -6.745008222462202774, 5.783357778048658027 ) ) ;
#3384 = EDGE_CURVE ( 'NONE', #7756, #13000, #10448, .T. ) ;
#3385 = EDGE_CURVE ( 'NONE', #1497, #9311, #14765, .T. ) ;
#3386 = ORIENTED_EDGE ( 'NONE', *, *, #10791, .F. ) ;
#3387 = CARTESIAN_POINT ( 'NONE',  ( 26.01652455409633902, -4.902371455920926380, -5.783357778048663356 ) ) ;
#3388 = CARTESIAN_POINT ( 'NONE',  ( 10.50000000000000000, 1.285879139104720831E-15, -2.000000000000000000 ) ) ;
#3389 = CARTESIAN_POINT ( 'NONE',  ( 0.000000000000000000, 0.000000000000000000, -8.700000000000001066 ) ) ;
#3390 = ORIENTED_EDGE ( 'NONE', *, *, #2959, .F. ) ;
#3391 = CARTESIAN_POINT ( 'NONE',  ( 26.24567459566274508, -6.804343261277824517, 4.147687604665191152 ) ) ;
#3392 = CARTESIAN_POINT ( 'NONE',  ( -27.17934203385504333, -30.00000000000000355, 12.00000000000000000 ) ) ;
#3393 = CIRCLE ( 'NONE', #8898, 12.50000000000000000 ) ;
#3394 = CARTESIAN_POINT ( 'NONE',  ( 20.00000000000000000, 7.999999999999996447, 15.51150668642334374 ) ) ;
#3395 = LINE ( 'NONE', #7572, #1842 ) ;
#3396 = ADVANCED_FACE ( 'NONE', ( #10195 ), #8766, .F. ) ;
#3397 = CARTESIAN_POINT ( 'NONE',  ( 29.89119874204131122, -2.254829357712824667, -4.533357778048659803 ) ) ;
#3398 = CARTESIAN_POINT ( 'NONE',  ( -27.17934203385504333, -30.00000000000000355, 13.93658524716016878 ) ) ;
#3399 = CARTESIAN_POINT ( 'NONE',  ( 26.31176419598820360, -7.352894575460818594, 5.384699358761103838 ) ) ;
#3400 = CARTESIAN_POINT ( 'NONE',  ( 29.80442540930208750, -6.953886339277345563, -5.783357778048669573 ) ) ;
#3401 = CARTESIAN_POINT ( 'NONE',  ( 27.19802975513453092, -2.241944418315925613, -5.783357778048658027 ) ) ;
#3402 = DIRECTION ( 'NONE',  ( -5.026720092345836698E-22, 4.581671729415424240E-22, -1.000000000000000000 ) ) ;
#3403 = CARTESIAN_POINT ( 'NONE',  ( 26.52522735095806894, -6.721994413439005278, 6.861505862736157368 ) ) ;
#3404 = VECTOR ( 'NONE', #7432, 1000.000000000000000 ) ;
#3405 = ORIENTED_EDGE ( 'NONE', *, *, #10870, .F. ) ;
#3406 = CARTESIAN_POINT ( 'NONE',  ( 25.62757597683262034, -3.695291012717980994, -7.939653947423660263 ) ) ;
#3407 = EDGE_CURVE ( 'NONE', #7967, #11475, #4755, .T. ) ;
#3408 = ORIENTED_EDGE ( 'NONE', *, *, #8081, .T. ) ;
#3409 = CARTESIAN_POINT ( 'NONE',  ( 32.70264286945147347, -5.350767304972614546, 7.939653947423658487 ) ) ;
#3410 = DIRECTION ( 'NONE',  ( 0.9928203230275512992, 0.1196152422706614898, -0.000000000000000000 ) ) ;
#3411 = VERTEX_POINT ( 'NONE', #17115 ) ;
#3412 = CARTESIAN_POINT ( 'NONE',  ( 45.00000000000000711, -16.03270077640482683, 0.5379818257722508434 ) ) ;
#3413 = CARTESIAN_POINT ( 'NONE',  ( -36.95907006869318678, -17.52584492564777818, -5.783357778048662468 ) ) ;
#3414 = CARTESIAN_POINT ( 'NONE',  ( 2.500000000000000000, 0.000000000000000000, 0.000000000000000000 ) ) ;
#3415 = EDGE_CURVE ( 'NONE', #1004, #6730, #14163, .T. ) ;
#3416 = CARTESIAN_POINT ( 'NONE',  ( 32.80318959510331212, -2.203800746085299522, -4.705209693361160461 ) ) ;
#3417 = ADVANCED_FACE ( 'NONE', ( #17672, #9286 ), #16375, .T. ) ;
#3418 =( BOUNDED_CURVE ( )  B_SPLINE_CURVE ( 2, ( #16214, #9043, #790, #9135, #881, #2429, #7771, #17418, #4772 ),
 .UNSPECIFIED., .F., .T. ) 
 B_SPLINE_CURVE_WITH_KNOTS ( ( 3, 2, 2, 2, 3 ),
 ( 0.2500000000000000000, 0.2564102564102563875, 0.2692307692307692180, 0.2820512820512820484, 0.2884615384615384914 ),
 .UNSPECIFIED. ) 
 CURVE ( )  GEOMETRIC_REPRESENTATION_ITEM ( )  RATIONAL_B_SPLINE_CURVE ( ( 0.9330127018922194093, 0.9330127018922195203, 1.000000000000000000, 0.8660254037844387076, 1.000000000000000000, 0.8660254037844387076, 1.000000000000000000, 0.9330127018922190762, 0.9330127018922194093 ) ) 
 REPRESENTATION_ITEM ( '' )  );
#3419 = CARTESIAN_POINT ( 'NONE',  ( 27.32822876973539294, -6.198150586942257512, -3.283357778048667797 ) ) ;
#3420 = MECHANICAL_DESIGN_GEOMETRIC_PRESENTATION_REPRESENTATION (  '', ( #8047 ), #235 ) ;
#3421 = CARTESIAN_POINT ( 'NONE',  ( 26.01652455409633902, -4.902371455920926380, 5.783357778048663356 ) ) ;
#3422 = FACE_OUTER_BOUND ( 'NONE', #8222, .T. ) ;
#3423 = CARTESIAN_POINT ( 'NONE',  ( 26.88845778707760914, -3.543379655034240905, -7.939653947423660263 ) ) ;
#3424 = EDGE_LOOP ( 'NONE', ( #10033, #5132, #2923, #10696 ) ) ;
#3425 = CARTESIAN_POINT ( 'NONE',  ( 32.06776442294927421, -4.173316554281249147, -3.283357778048664688 ) ) ;
#3426 = VECTOR ( 'NONE', #5263, 1000.000000000000000 ) ;
#3427 = CARTESIAN_POINT ( 'NONE',  ( 31.71123609653335507, -2.762457591843783256, 3.283357778048666464 ) ) ;
#3428 = VERTEX_POINT ( 'NONE', #13472 ) ;
#3429 = ORIENTED_EDGE ( 'NONE', *, *, #14396, .F. ) ;
#3430 = AXIS2_PLACEMENT_3D ( 'NONE', #1199, #10952, #8080 ) ;
#3431 = EDGE_CURVE ( 'NONE', #4898, #9735, #7354, .T. ) ;
#3432 = VERTEX_POINT ( 'NONE', #1229 ) ;
#3433 = LINE ( 'NONE', #9056, #10629 ) ;
#3434 = AXIS2_PLACEMENT_3D ( 'NONE', #1063, #9390, #17867 ) ;
#3435 = CARTESIAN_POINT ( 'NONE',  ( 33.13163345120441505, -4.045141346131868154, 7.939653947423662039 ) ) ;
#3436 = DIRECTION ( 'NONE',  ( -0.000000000000000000, 0.000000000000000000, -1.000000000000000000 ) ) ;
#3437 = DIRECTION ( 'NONE',  ( 0.000000000000000000, 0.000000000000000000, -1.000000000000000000 ) ) ;
#3438 = FACE_OUTER_BOUND ( 'NONE', #1317, .T. ) ;
#3439 = CARTESIAN_POINT ( 'NONE',  ( 32.95662993491455950, -6.574107945067995118, -5.783357778048669573 ) ) ;
#3440 = CARTESIAN_POINT ( 'NONE',  ( 31.34233605952372415, -6.778795339760710803, -5.783357778048663356 ) ) ;
#3441 = LINE ( 'NONE', #2098, #6686 ) ;
#3442 = ORIENTED_EDGE ( 'NONE', *, *, #7326, .T. ) ;
#3443 = CARTESIAN_POINT ( 'NONE',  ( -2.805705207896067588, 3.226868319750155756, -3.203898532754366979 ) ) ;
#3444 = CARTESIAN_POINT ( 'NONE',  ( 27.32822876973539294, -6.198150586942257512, -3.283357778048667797 ) ) ;
#3445 =( BOUNDED_CURVE ( )  B_SPLINE_CURVE ( 2, ( #484, #10168, #10070, #5993, #11519, #6090, #17088, #1857, #15720 ),
 .UNSPECIFIED., .F., .T. ) 
 B_SPLINE_CURVE_WITH_KNOTS ( ( 3, 2, 2, 2, 3 ),
 ( 0.5961538461538461453, 0.6025641025641025328, 0.6153846153846154188, 0.6282051282051281937, 0.6346153846153846922 ),
 .UNSPECIFIED. ) 
 CURVE ( )  GEOMETRIC_REPRESENTATION_ITEM ( )  RATIONAL_B_SPLINE_CURVE ( ( 0.9330127018922194093, 0.9330127018922194093, 1.000000000000000000, 0.8660254037844387076, 1.000000000000000000, 0.8660254037844387076, 1.000000000000000000, 0.9330127018922187432, 0.9330127018922192983 ) ) 
 REPRESENTATION_ITEM ( '' )  );
#3446 = CARTESIAN_POINT ( 'NONE',  ( 26.61898274975073164, -6.283600725846810953, -3.283357778048667797 ) ) ;
#3447 = VERTEX_POINT ( 'NONE', #958 ) ;
#3448 = VECTOR ( 'NONE', #7975, 1000.000000000000114 ) ;
#3449 = EDGE_CURVE ( 'NONE', #8791, #13340, #10643, .T. ) ;
#3450 = CARTESIAN_POINT ( 'NONE',  ( 28.25893984004492765, -6.513116296623863377, -4.705209693361168455 ) ) ;
#3451 = CARTESIAN_POINT ( 'NONE',  ( 32.29974222271236073, -2.891426744974864071, -3.627061608673662008 ) ) ;
#3452 =( REPRESENTATION_RELATIONSHIP ('NONE','NONE', #3227, #3339 ) REPRESENTATION_RELATIONSHIP_WITH_TRANSFORMATION ( #2234 )SHAPE_REPRESENTATION_RELATIONSHIP( ) );
#3453 = EDGE_LOOP ( 'NONE', ( #17654, #12272, #10983, #8467 ) ) ;
#3454 = CARTESIAN_POINT ( 'NONE',  ( 0.000000000000000000, 0.000000000000000000, 1.159999999999999476 ) ) ;
#3455 = CARTESIAN_POINT ( 'NONE',  ( 29.04309111455793513, -1.630102785574754742, 5.783357778048668685 ) ) ;
#3456 =( BOUNDED_SURFACE ( )  B_SPLINE_SURFACE ( 1, 2, ( 
 ( #8565, #4485, #12641, #17016, #10091, #3044, #11539, #8660, #14015, #4661, #139, #12915, #4569, #2950, #6013, #9817, #14098, #15640, #3218, #1598, #1684, #8760, #10189, #11254, #7040, #7130, #14290, #1876, #7405, #14189, #1781, #1506, #15738, #5833, #11357, #231, #7220, #12555, #11163, #5741, #16832, #3127, #4397, #9911, #15460, #12730, #7312, #327, #15543, #9999, #12830, #421, #15822, #6113, #17296, #4833, #11815, #6294, #13006, #13369, #854, #8841, #3397, #11641, #13103, #8926, #7665, #17580, #7745, #2232, #952, #5019, #14469, #10541, #3666, #11906, #17206, #5100, #6206, #14649, #10620, #4748, #1960, #6484, #10361, #680, #2050, #13190, #7575, #11725, #14378, #16105, #16193, #7839, #17394, #10274, #15915, #3487, #4925, #10455, #589, #11999, #6386, #7480, #9021, #14570, #2148, #767, #16015, #3588, #13274, #17493, #9111, #9192, #14736, #2324, #16532, #6827, #1040, #12444, #1122, #9535, #30, #17665, #14819, #13804, #5279, #8008, #14903, #2572, #2486, #16281, #9278, #17921, #5540, #2754, #1221, #6738, #16371, #6560, #10972, #16450, #1390, #8099, #11065, #2409, #12080, #10706, #3852, #5188, #6912, #4019, #1306 ),
 ( #3757, #9448, #8195, #12274, #17753, #17842, #13547, #15080, #7931, #6647, #13465, #9363, #3934, #5362, #12175, #13721, #5452, #10795, #14986, #2664, #13633, #10881, #12353, #8273, #4112, #9621, #15173, #12536, #16811, #1756, #5904, #4286, #4377, #11428, #14265, #13995, #9703, #11144, #8635, #398, #10068, #16909, #4463, #4203, #16992, #8546, #14078, #1482, #5717, #481, #15253, #7012, #5628, #5810, #14165, #5990, #12803, #7286, #11331, #7383, #301, #9889, #4548, #15441, #16714, #9793, #1664, #1578, #13891, #7198, #120, #15617, #7111, #12625, #3106, #16626, #2924, #3195, #8734, #1854, #15345, #8458, #12898, #2830, #9978, #8360, #208, #11234, #3023, #12708, #15525, #17467, #14446, #13351, #4998, #6183, #10165, #4729, #7461, #3293, #14718, #929, #9091, #14355, #10341, #8910, #3654, #2302, #12985, #10253, #1941, #747, #7820, #570, #4907, #11516, #2029, #9174, #11705, #3566, #6274, #14633, #10435, #15994, #11794, #2214, #8824, #17085, #7552, #17276, #836, #6089, #4812, #13076, #4640, #15718, #11617, #15894, #3468, #17182, #7727, #13254, #6365, #15802, #11888, #10525, #16086, #3377, #660, #8999, #17373, #14544, #2126 ) ),
 .UNSPECIFIED., .F., .F., .T. ) 
 B_SPLINE_SURFACE_WITH_KNOTS ( ( 2, 2 ),
 ( 3, 2, 2, 2, 2, 2, 2, 2, 2, 2, 2, 2, 2, 2, 2, 2, 2, 2, 2, 2, 2, 2, 2, 2, 2, 2, 2, 2, 2, 2, 2, 2, 2, 2, 2, 2, 2, 2, 2, 2, 2, 2, 2, 2, 2, 2, 2, 2, 2, 2, 2, 2, 2, 2, 2, 2, 2, 2, 2, 2, 2, 2, 2, 2, 2, 2, 2, 2, 2, 2, 2, 2, 2, 2, 2, 2, 3 ),
 ( 0.000000000000000000, 1.000000000000000000 ),
 ( 0.000000000000000000, 0.01282051282051282007, 0.02564102564102564014, 0.03846153846153846367, 0.05128205128205128027, 0.06410256410256409687, 0.07692307692307692735, 0.08974358974358974395, 0.1025641025641025605, 0.1153846153846153910, 0.1282051282051281937, 0.1410256410256410242, 0.1538461538461538547, 0.1666666666666666574, 0.1794871794871794879, 0.1923076923076923184, 0.2051282051282051211, 0.2179487179487179516, 0.2307692307692307820, 0.2435897435897435848, 0.2564102564102563875, 0.2692307692307692180, 0.2820512820512820484, 0.2948717948717948789, 0.3076923076923077094, 0.3205128205128205399, 0.3333333333333333148, 0.3461538461538461453, 0.3589743589743589758, 0.3717948717948718063, 0.3846153846153846367, 0.3974358974358974117, 0.4102564102564102422, 0.4230769230769230727, 0.4358974358974359031, 0.4487179487179487336, 0.4615384615384615641, 0.4743589743589743390, 0.4871794871794871695, 0.5000000000000000000, 0.5128205128205127750, 0.5256410256410256610, 0.5384615384615384359, 0.5512820512820513219, 0.5641025641025640969, 0.5769230769230768718, 0.5897435897435897578, 0.6025641025641025328, 0.6153846153846154188, 0.6282051282051281937, 0.6410256410256410797, 0.6538461538461538547, 0.6666666666666666297, 0.6794871794871795156, 0.6923076923076922906, 0.7051282051282051766, 0.7179487179487179516, 0.7307692307692307265, 0.7435897435897436125, 0.7564102564102563875, 0.7692307692307692735, 0.7820512820512820484, 0.7948717948717948234, 0.8076923076923077094, 0.8205128205128204844, 0.8333333333333333703, 0.8461538461538461453, 0.8589743589743589203, 0.8717948717948718063, 0.8846153846153845812, 0.8974358974358974672, 0.9102564102564102422, 0.9230769230769231282, 0.9358974358974359031, 0.9487179487179486781, 0.9615384615384615641, 0.9690837704703162414 ),
 .UNSPECIFIED. ) 
 GEOMETRIC_REPRESENTATION_ITEM ( )  RATIONAL_B_SPLINE_SURFACE ( (
 ( 1.000000000000000000, 0.8660254037844387076, 1.000000000000000000, 0.8660254037844387076, 1.000000000000000000, 0.8660254037844387076, 1.000000000000000000, 0.8660254037844387076, 1.000000000000000000, 0.8660254037844387076, 1.000000000000000000, 0.8660254037844387076, 1.000000000000000000, 0.8660254037844387076, 1.000000000000000000, 0.8660254037844387076, 1.000000000000000000, 0.8660254037844387076, 1.000000000000000000, 0.8660254037844387076, 1.000000000000000000, 0.8660254037844387076, 1.000000000000000000, 0.8660254037844387076, 1.000000000000000000, 0.8660254037844387076, 1.000000000000000000, 0.8660254037844387076, 1.000000000000000000, 0.8660254037844387076, 1.000000000000000000, 0.8660254037844387076, 1.000000000000000000, 0.8660254037844387076, 1.000000000000000000, 0.8660254037844387076, 1.000000000000000000, 0.8660254037844387076, 1.000000000000000000, 0.8660254037844387076, 1.000000000000000000, 0.8660254037844387076, 1.000000000000000000, 0.8660254037844387076, 1.000000000000000000, 0.8660254037844387076, 1.000000000000000000, 0.8660254037844387076, 1.000000000000000000, 0.8660254037844387076, 1.000000000000000000, 0.8660254037844387076, 1.000000000000000000, 0.8660254037844387076, 1.000000000000000000, 0.8660254037844387076, 1.000000000000000000, 0.8660254037844387076, 1.000000000000000000, 0.8660254037844387076, 1.000000000000000000, 0.8660254037844387076, 1.000000000000000000, 0.8660254037844387076, 1.000000000000000000, 0.8660254037844387076, 1.000000000000000000, 0.8660254037844387076, 1.000000000000000000, 0.8660254037844387076, 1.000000000000000000, 0.8660254037844387076, 1.000000000000000000, 0.8660254037844387076, 1.000000000000000000, 0.8660254037844387076, 1.000000000000000000, 0.8660254037844387076, 1.000000000000000000, 0.8660254037844387076, 1.000000000000000000, 0.8660254037844387076, 1.000000000000000000, 0.8660254037844387076, 1.000000000000000000, 0.8660254037844387076, 1.000000000000000000, 0.8660254037844387076, 1.000000000000000000, 0.8660254037844387076, 1.000000000000000000, 0.8660254037844387076, 1.000000000000000000, 0.8660254037844387076, 1.000000000000000000, 0.8660254037844387076, 1.000000000000000000, 0.8660254037844387076, 1.000000000000000000, 0.8660254037844387076, 1.000000000000000000, 0.8660254037844387076, 1.000000000000000000, 0.8660254037844387076, 1.000000000000000000, 0.8660254037844387076, 1.000000000000000000, 0.8660254037844387076, 1.000000000000000000, 0.8660254037844387076, 1.000000000000000000, 0.8660254037844387076, 1.000000000000000000, 0.8660254037844387076, 1.000000000000000000, 0.8660254037844387076, 1.000000000000000000, 0.8660254037844387076, 1.000000000000000000, 0.8660254037844387076, 1.000000000000000000, 0.8660254037844387076, 1.000000000000000000, 0.8660254037844387076, 1.000000000000000000, 0.8660254037844387076, 1.000000000000000000, 0.8660254037844387076, 1.000000000000000000, 0.8660254037844387076, 1.000000000000000000, 0.8660254037844387076, 1.000000000000000000, 0.8660254037844387076, 1.000000000000000000, 0.8660254037844387076, 1.000000000000000000, 0.8660254037844387076, 1.000000000000000000, 0.8660254037844387076, 1.000000000000000000, 0.8660254037844387076, 1.000000000000000000, 0.8660254037844387076, 1.000000000000000000, 0.8660254037844387076, 1.000000000000000000, 0.8660254037844387076, 1.000000000000000000, 0.8660254037844387076, 1.000000000000000000, 0.9211513820375816231, 0.9351129643698559146),
 ( 1.000000000000000000, 0.8660254037844387076, 1.000000000000000000, 0.8660254037844387076, 1.000000000000000000, 0.8660254037844387076, 1.000000000000000000, 0.8660254037844387076, 1.000000000000000000, 0.8660254037844387076, 1.000000000000000000, 0.8660254037844387076, 1.000000000000000000, 0.8660254037844387076, 1.000000000000000000, 0.8660254037844387076, 1.000000000000000000, 0.8660254037844387076, 1.000000000000000000, 0.8660254037844387076, 1.000000000000000000, 0.8660254037844387076, 1.000000000000000000, 0.8660254037844387076, 1.000000000000000000, 0.8660254037844387076, 1.000000000000000000, 0.8660254037844387076, 1.000000000000000000, 0.8660254037844387076, 1.000000000000000000, 0.8660254037844387076, 1.000000000000000000, 0.8660254037844387076, 1.000000000000000000, 0.8660254037844387076, 1.000000000000000000, 0.8660254037844387076, 1.000000000000000000, 0.8660254037844387076, 1.000000000000000000, 0.8660254037844387076, 1.000000000000000000, 0.8660254037844387076, 1.000000000000000000, 0.8660254037844387076, 1.000000000000000000, 0.8660254037844387076, 1.000000000000000000, 0.8660254037844387076, 1.000000000000000000, 0.8660254037844387076, 1.000000000000000000, 0.8660254037844387076, 1.000000000000000000, 0.8660254037844387076, 1.000000000000000000, 0.8660254037844387076, 1.000000000000000000, 0.8660254037844387076, 1.000000000000000000, 0.8660254037844387076, 1.000000000000000000, 0.8660254037844387076, 1.000000000000000000, 0.8660254037844387076, 1.000000000000000000, 0.8660254037844387076, 1.000000000000000000, 0.8660254037844387076, 1.000000000000000000, 0.8660254037844387076, 1.000000000000000000, 0.8660254037844387076, 1.000000000000000000, 0.8660254037844387076, 1.000000000000000000, 0.8660254037844387076, 1.000000000000000000, 0.8660254037844387076, 1.000000000000000000, 0.8660254037844387076, 1.000000000000000000, 0.8660254037844387076, 1.000000000000000000, 0.8660254037844387076, 1.000000000000000000, 0.8660254037844387076, 1.000000000000000000, 0.8660254037844387076, 1.000000000000000000, 0.8660254037844387076, 1.000000000000000000, 0.8660254037844387076, 1.000000000000000000, 0.8660254037844387076, 1.000000000000000000, 0.8660254037844387076, 1.000000000000000000, 0.8660254037844387076, 1.000000000000000000, 0.8660254037844387076, 1.000000000000000000, 0.8660254037844387076, 1.000000000000000000, 0.8660254037844387076, 1.000000000000000000, 0.8660254037844387076, 1.000000000000000000, 0.8660254037844387076, 1.000000000000000000, 0.8660254037844387076, 1.000000000000000000, 0.8660254037844387076, 1.000000000000000000, 0.8660254037844387076, 1.000000000000000000, 0.8660254037844387076, 1.000000000000000000, 0.8660254037844387076, 1.000000000000000000, 0.8660254037844387076, 1.000000000000000000, 0.8660254037844387076, 1.000000000000000000, 0.8660254037844387076, 1.000000000000000000, 0.8660254037844387076, 1.000000000000000000, 0.8660254037844387076, 1.000000000000000000, 0.8660254037844387076, 1.000000000000000000, 0.8660254037844387076, 1.000000000000000000, 0.8660254037844387076, 1.000000000000000000, 0.8660254037844387076, 1.000000000000000000, 0.8660254037844387076, 1.000000000000000000, 0.8660254037844387076, 1.000000000000000000, 0.8660254037844387076, 1.000000000000000000, 0.8660254037844387076, 1.000000000000000000, 0.8660254037844387076, 1.000000000000000000, 0.8660254037844387076, 1.000000000000000000, 0.9211513820375816231, 0.9351129643698559146) ) ) 
 REPRESENTATION_ITEM ( '' )  SURFACE ( )  );
#3457 = ORIENTED_EDGE ( 'NONE', *, *, #47, .T. ) ;
#3458 = CARTESIAN_POINT ( 'NONE',  ( 26.15738093914773543, -4.885401043216321959, 3.283357778048664244 ) ) ;
#3459 = CARTESIAN_POINT ( 'NONE',  ( 30.12381574833269937, -2.526612381163247267, -4.705209693361161349 ) ) ;
#3460 = ORIENTED_EDGE ( 'NONE', *, *, #17909, .T. ) ;
#3461 = AXIS2_PLACEMENT_3D ( 'NONE', #15762, #11282, #4331 ) ;
#3462 = CARTESIAN_POINT ( 'NONE',  ( 29.18195272205665347, -2.340279496617377664, -4.533357778048659803 ) ) ;
#3463 = CARTESIAN_POINT ( 'NONE',  ( 32.87199790123699472, -1.558343308739095656, -5.783357778048663356 ) ) ;
#3464 = DIRECTION ( 'NONE',  ( -0.000000000000000000, -0.000000000000000000, -1.000000000000000000 ) ) ;
#3465 = CARTESIAN_POINT ( 'NONE',  ( 28.08810621022444920, -4.652786776866828511, -3.627061608673664672 ) ) ;
#3466 = VECTOR ( 'NONE', #2832, 1000.000000000000000 ) ;
#3467 = EDGE_CURVE ( 'NONE', #3702, #8474, #407, .T. ) ;
#3468 = CARTESIAN_POINT ( 'NONE',  ( 26.35439372113758694, -4.861664893681965083, -7.939653947423662039 ) ) ;
#3469 = CARTESIAN_POINT ( 'NONE',  ( 28.09001152836988524, -6.106370808549102414, -8.283357778048664244 ) ) ;
#3470 = LINE ( 'NONE', #13173, #10402 ) ;
#3471 = CARTESIAN_POINT ( 'NONE',  ( -2.500000000000000000, 3.061616997868383141E-16, -10.00000000000000000 ) ) ;
#3472 = CARTESIAN_POINT ( 'NONE',  ( 27.92107091181166467, -2.492190854301117753, -4.533357778048659803 ) ) ;
#3473 = VECTOR ( 'NONE', #2224, 1000.000000000000000 ) ;
#3474 = DIRECTION ( 'NONE',  ( 0.000000000000000000, 0.000000000000000000, -1.000000000000000000 ) ) ;
#3475 = EDGE_CURVE ( 'NONE', #16224, #63, #8851, .T. ) ;
#3476 = ORIENTED_EDGE ( 'NONE', *, *, #826, .T. ) ;
#3477 = CARTESIAN_POINT ( 'NONE',  ( -4.101948962585904468, 2.368261337751077722, -3.381124513963622569 ) ) ;
#3478 = CARTESIAN_POINT ( 'NONE',  ( 26.95740407890011170, -7.307093047852763590, -6.453230759126468818 ) ) ;
#3479 = CARTESIAN_POINT ( 'NONE',  ( 8.632250723006720250, -18.84644399697197770, -16.84735068286506987 ) ) ;
#3480 = EDGE_LOOP ( 'NONE', ( #7545, #2766, #493, #13060 ) ) ;
#3481 = LINE ( 'NONE', #15633, #9615 ) ;
#3482 = CARTESIAN_POINT ( 'NONE',  ( 39.99999999999999289, 0.000000000000000000, 0.000000000000000000 ) ) ;
#3483 = CARTESIAN_POINT ( 'NONE',  ( 45.50000000000000000, -16.03270077640482683, -2.787981825772262390 ) ) ;
#3484 = CARTESIAN_POINT ( 'NONE',  ( 33.54323074294813267, -5.249493066516778050, -7.939653947423662927 ) ) ;
#3485 = DIRECTION ( 'NONE',  ( 1.000000000000000000, 0.000000000000000000, 0.000000000000000000 ) ) ;
#3486 = EDGE_CURVE ( 'NONE', #9702, #17832, #15294, .T. ) ;
#3487 = CARTESIAN_POINT ( 'NONE',  ( 28.13873763417254992, -3.192873105281056390, -3.283357778048662023 ) ) ;
#3488 = DIRECTION ( 'NONE',  ( 0.000000000000000000, 0.000000000000000000, -1.000000000000000000 ) ) ;
#3489 = VECTOR ( 'NONE', #15521, 1000.000000000000114 ) ;
#3490 = EDGE_CURVE ( 'NONE', #4413, #3428, #1995, .T. ) ;
#3491 = CONTEXT_DEPENDENT_SHAPE_REPRESENTATION ( #10020, #6642 ) ;
#3492 = DIRECTION ( 'NONE',  ( 0.9928203230275512992, 0.1196152422706610180, 4.006172263299093133E-17 ) ) ;
#3493 = CARTESIAN_POINT ( 'NONE',  ( 30.28142597461332741, -2.507623461452779701, -4.705209693361160461 ) ) ;
#3494 = DIRECTION ( 'NONE',  ( 0.000000000000000000, 0.000000000000000000, 1.000000000000000000 ) ) ;
#3495 = CARTESIAN_POINT ( 'NONE',  ( 26.01652455409633902, -4.902371455920928156, -5.783357778048663356 ) ) ;
#3496 = CARTESIAN_POINT ( 'NONE',  ( 28.41655006632555569, -6.494127376913395366, 6.861505862736157368 ) ) ;
#3497 = VERTEX_POINT ( 'NONE', #9367 ) ;
#3498 = EDGE_LOOP ( 'NONE', ( #17288, #16593, #4447, #7418 ) ) ;
#3499 = CARTESIAN_POINT ( 'NONE',  ( 26.87106449706838873, -6.053357334259913181, -3.627061608673667781 ) ) ;
#3500 = ORIENTED_EDGE ( 'NONE', *, *, #17256, .F. ) ;
#3501 = CARTESIAN_POINT ( 'NONE',  ( 25.60565592828815440, -3.070961412863312034, 4.705209693361167567 ) ) ;
#3502 =( NAMED_UNIT ( * ) SI_UNIT ( $, .STERADIAN. ) SOLID_ANGLE_UNIT ( ) );
#3503 = CARTESIAN_POINT ( 'NONE',  ( 27.45957062324739084, -6.182326487390971792, -8.283357778048664244 ) ) ;
#3504 = ORIENTED_EDGE ( 'NONE', *, *, #6011, .T. ) ;
#3505 = AXIS2_PLACEMENT_3D ( 'NONE', #14357, #12986, #571 ) ;
#3506 = DIRECTION ( 'NONE',  ( 1.000000000000000000, 0.000000000000000000, 0.000000000000000000 ) ) ;
#3507 = CARTESIAN_POINT ( 'NONE',  ( 30.64556327217151122, -6.525384084031224496, 4.533357778048659803 ) ) ;
#3508 = PLANE ( 'NONE',  #8769 ) ;
#3509 = CARTESIAN_POINT ( 'NONE',  ( 31.97277696464621854, -6.702839660918840536, -5.783357778048663356 ) ) ;
#3510 = AXIS2_PLACEMENT_3D ( 'NONE', #13787, #14141, #7176 ) ;
#3511 = CARTESIAN_POINT ( 'NONE',  ( 32.75517961154501023, -5.344437665069116328, -7.939653947423664704 ) ) ;
#3512 = CARTESIAN_POINT ( 'NONE',  ( 28.45891156537951971, -2.090033060632186412, -5.783357778048670461 ) ) ;
#3513 = DIRECTION ( 'NONE',  ( 0.000000000000000000, 0.000000000000000000, 1.000000000000000000 ) ) ;
#3514 = CARTESIAN_POINT ( 'NONE',  ( 26.45077056032005913, -6.103994453487816330, -7.939653947423664704 ) ) ;
#3515 = EDGE_CURVE ( 'NONE', #15247, #11836, #1045, .T. ) ;
#3516 = DIRECTION ( 'NONE',  ( 0.9928203230275510771, 0.1196152422706614621, -0.000000000000000000 ) ) ;
#3517 = CARTESIAN_POINT ( 'NONE',  ( 31.24973580796908834, -6.452593224933654170, 7.033357778048657138 ) ) ;
#3518 = ORIENTED_EDGE ( 'NONE', *, *, #9994, .F. ) ;
#3519 = EDGE_CURVE ( 'NONE', #16712, #3946, #9186, .T. ) ;
#3520 = VERTEX_POINT ( 'NONE', #14744 ) ;
#3521 = CIRCLE ( 'NONE', #626, 2.700000000000000622 ) ;
#3522 = VERTEX_POINT ( 'NONE', #2577 ) ;
#3523 = CYLINDRICAL_SURFACE ( 'NONE', #14981, 2.499999999999999112 ) ;
#3524 = CARTESIAN_POINT ( 'NONE',  ( 32.17274868998081416, -2.279756424927169345, 6.861505862736166250 ) ) ;
#3525 = ORIENTED_EDGE ( 'NONE', *, *, #17843, .F. ) ;
#3526 =( BOUNDED_CURVE ( )  B_SPLINE_CURVE ( 2, ( #5489, #4157, #17875, #5399, #17619, #9654, #9485, #15025, #2445 ),
 .UNSPECIFIED., .F., .T. ) 
 B_SPLINE_CURVE_WITH_KNOTS ( ( 3, 2, 2, 2, 3 ),
 ( 0.3269230769230769273, 0.3333333333333333148, 0.3461538461538461453, 0.3589743589743589758, 0.3653846153846154188 ),
 .UNSPECIFIED. ) 
 CURVE ( )  GEOMETRIC_REPRESENTATION_ITEM ( )  RATIONAL_B_SPLINE_CURVE ( ( 0.9330127018922194093, 0.9330127018922194093, 1.000000000000000000, 0.8660254037844387076, 1.000000000000000000, 0.8660254037844387076, 1.000000000000000000, 0.9330127018922190762, 0.9330127018922194093 ) ) 
 REPRESENTATION_ITEM ( '' )  );
#3527 = SURFACE_SIDE_STYLE ('',( #6430 ) ) ;
#3528 = CARTESIAN_POINT ( 'NONE',  ( 29.81991338116587542, -2.990324628369393611, -8.283357778048660691 ) ) ;
#3529 = CARTESIAN_POINT ( 'NONE',  ( -22.62145100412528009, -22.46994790986326151, -15.00472644746570694 ) ) ;
#3531 = AXIS2_PLACEMENT_3D ( 'NONE', #2482, #10701, #17662 ) ;
#3530 = CARTESIAN_POINT ( 'NONE',  ( 29.03376756790819613, -4.538853258604016006, -7.939653947423662039 ) ) ;
#3532 = CARTESIAN_POINT ( 'NONE',  ( 38.15053902264412500, -1.114360604510109765, -9.783357778048662468 ) ) ;
#3533 = CARTESIAN_POINT ( 'NONE',  ( 15.92260893619738837, -28.39189527176317540, 12.00000000000000000 ) ) ;
#3534 = VECTOR ( 'NONE', #16708, 1000.000000000000000 ) ;
#3535 = CARTESIAN_POINT ( 'NONE',  ( 14.05146698326616672, 13.69412420653798357, 16.38624388364804219 ) ) ;
#3536 = CARTESIAN_POINT ( 'NONE',  ( 31.05948030073166066, -1.776715885202022394, -5.783357778048662468 ) ) ;
#3537 = CARTESIAN_POINT ( 'NONE',  ( 35.77680296528374271, -19.03270077640483038, 0.5379818257722512875 ) ) ;
#3538 = VECTOR ( 'NONE', #15938, 1000.000000000000000 ) ;
#3539 = ORIENTED_EDGE ( 'NONE', *, *, #3647, .T. ) ;
#3540 = AXIS2_PLACEMENT_3D ( 'NONE', #544, #16784, #14056 ) ;
#3541 = EDGE_LOOP ( 'NONE', ( #17775, #2844, #8174, #16645 ) ) ;
#3542 = EDGE_CURVE ( 'NONE', #11419, #8674, #9475, .T. ) ;
#3543 = CARTESIAN_POINT ( 'NONE',  ( 26.88845778707760914, -3.543379655034240905, -7.939653947423660263 ) ) ;
#3544 = CARTESIAN_POINT ( 'NONE',  ( 31.69574812466957781, -6.726019302751734763, -5.783357778048669573 ) ) ;
#3545 = ORIENTED_EDGE ( 'NONE', *, *, #7913, .F. ) ;
#3546 = CYLINDRICAL_SURFACE ( 'NONE', #8058, 2.499999999999999112 ) ;
#3547 = CARTESIAN_POINT ( 'NONE',  ( 31.61111609099199171, -1.710254666422835745, -5.783357778048662468 ) ) ;
#3548 = EDGE_CURVE ( 'NONE', #8691, #17122, #15328, .T. ) ;
#3549 = ORIENTED_EDGE ( 'NONE', *, *, #698, .F. ) ;
#3550 = PLANE ( 'NONE',  #12971 ) ;
#3551 = CARTESIAN_POINT ( 'NONE',  ( 31.30154412293507349, -3.011689903141150815, -7.939653947423660263 ) ) ;
#3552 = ORIENTED_EDGE ( 'NONE', *, *, #14065, .T. ) ;
#3553 = AXIS2_PLACEMENT_3D ( 'NONE', #4576, #12737, #4311 ) ;
#3554 = AXIS2_PLACEMENT_3D ( 'NONE', #6267, #14796, #11882 ) ;
#3555 =( BOUNDED_CURVE ( )  B_SPLINE_CURVE ( 2, ( #7000, #10467, #2479, #6636, #6820, #8186, #2562, #21, #15163 ),
 .UNSPECIFIED., .F., .T. ) 
 B_SPLINE_CURVE_WITH_KNOTS ( ( 3, 2, 2, 2, 3 ),
 ( 0.09615384615384617306, 0.1025641025641025605, 0.1153846153846153910, 0.1282051282051281937, 0.1346153846153846367 ),
 .UNSPECIFIED. ) 
 CURVE ( )  GEOMETRIC_REPRESENTATION_ITEM ( )  RATIONAL_B_SPLINE_CURVE ( ( 0.9330127018922194093, 0.9330127018922196314, 1.000000000000000000, 0.8660254037844387076, 1.000000000000000000, 0.8660254037844387076, 1.000000000000000000, 0.9330127018922190762, 0.9330127018922194093 ) ) 
 REPRESENTATION_ITEM ( '' )  );
#3556 = EDGE_CURVE ( 'NONE', #17384, #13349, #3393, .T. ) ;
#3557 = ORIENTED_EDGE ( 'NONE', *, *, #15558, .T. ) ;
#3558 = DIRECTION ( 'NONE',  ( -1.000000000000000000, 0.000000000000000000, 0.000000000000000000 ) ) ;
#3559 = CARTESIAN_POINT ( 'NONE',  ( 25.84832697747033592, -3.506312147857040706, -7.581167935121603918 ) ) ;
#3560 = DIRECTION ( 'NONE',  ( -1.000000000000000000, 0.000000000000000000, 0.000000000000000000 ) ) ;
#3561 = DIRECTION ( 'NONE',  ( -5.026720092345836698E-22, 4.581671729415424240E-22, -1.000000000000000000 ) ) ;
#3562 = VECTOR ( 'NONE', #871, 1000.000000000000227 ) ;
#3563 = CARTESIAN_POINT ( 'NONE',  ( 32.33415724766913257, -1.960501102408027219, -4.533357778048659803 ) ) ;
#3564 = EDGE_CURVE ( 'NONE', #11059, #15493, #9709, .T. ) ;
#3565 = VECTOR ( 'NONE', #13907, 1000.000000000000227 ) ;
#3566 = CARTESIAN_POINT ( 'NONE',  ( 27.50150540219088313, -5.977401655418042914, -3.627061608673667781 ) ) ;
#3567 = CARTESIAN_POINT ( 'NONE',  ( 25.95642634701329499, -4.403549397486667516, -3.686412874245489135 ) ) ;
#3568 = CARTESIAN_POINT ( 'NONE',  ( 37.96876116389215383, 4.574485896386907058, -9.283357778048655362 ) ) ;
#3569 = AXIS2_PLACEMENT_3D ( 'NONE', #13910, #17859, #5649 ) ;
#3570 = LINE ( 'NONE', #3471, #8184 ) ;
#3571 = ORIENTED_EDGE ( 'NONE', *, *, #9985, .T. ) ;
#3572 = CARTESIAN_POINT ( 'NONE',  ( 26.70901672940806648, -4.818939824437135755, -8.283357778048662468 ) ) ;
#3573 = CARTESIAN_POINT ( 'NONE',  ( 33.38562051666750818, -5.268481986227246949, -7.939653947423662927 ) ) ;
#3574 = AXIS2_PLACEMENT_3D ( 'NONE', #13937, #4592, #7063 ) ;
#3575 = AXIS2_PLACEMENT_3D ( 'NONE', #5095, #17575, #9272 ) ;
#3576 = EDGE_CURVE ( 'NONE', #10379, #15769, #6867, .T. ) ;
#3577 = ORIENTED_EDGE ( 'NONE', *, *, #11050, .T. ) ;
#3578 = FACE_OUTER_BOUND ( 'NONE', #7252, .T. ) ;
#3579 = CARTESIAN_POINT ( 'NONE',  ( 9.099998387031005720, -19.29508120620799971, -6.000000000000000000 ) ) ;
#3580 = CARTESIAN_POINT ( 'NONE',  ( -2.038300084272748336E-14, -4.618802153517010289, -0.5000000000000000000 ) ) ;
#3581 = COLOUR_RGB ( '', 0.09019608, 0.27058824, 0.51372549) ;
#3582 = ORIENTED_EDGE ( 'NONE', *, *, #16826, .F. ) ;
#3583 = FACE_OUTER_BOUND ( 'NONE', #15071, .T. ) ;
#3584 = FACE_OUTER_BOUND ( 'NONE', #16093, .T. ) ;
#3585 = CARTESIAN_POINT ( 'NONE',  ( 32.19919549706052209, -6.038393303862174655, -4.705209693361169343 ) ) ;
#3586 = DIRECTION ( 'NONE',  ( 0.1196152422706596996, -0.9928203230275514102, 0.000000000000000000 ) ) ;
#3587 = EDGE_CURVE ( 'NONE', #11980, #9649, #11015, .T. ) ;
#3588 = CARTESIAN_POINT ( 'NONE',  ( 27.50829672905005907, -3.268828784122927100, -3.283357778048662023 ) ) ;
#3589 = DIRECTION ( 'NONE',  ( 1.000000000000000000, 0.000000000000000000, 0.000000000000000000 ) ) ;
#3590 = ITEM_DEFINED_TRANSFORMATION ( 'NONE', 'NONE', #10563,  #3575 ) ;
#3591 = LINE ( 'NONE', #593, #14463 ) ;
#3592 = FACE_OUTER_BOUND ( 'NONE', #10283, .T. ) ;
#3593 = CARTESIAN_POINT ( 'NONE',  ( 28.39010325924584421, -2.735490497978389612, -4.705209693361160461 ) ) ;
#3594 = VECTOR ( 'NONE', #2654, 1000.000000000000000 ) ;
#3595 = DIRECTION ( 'NONE',  ( -0.000000000000000000, -0.000000000000000000, 1.000000000000000000 ) ) ;
#3596 = CARTESIAN_POINT ( 'NONE',  ( 33.53059316159333036, -1.478995586096186088, 6.453230759126471483 ) ) ;
#3597 =( GEOMETRIC_REPRESENTATION_CONTEXT ( 3 ) GLOBAL_UNCERTAINTY_ASSIGNED_CONTEXT ( ( #9343 ) ) GLOBAL_UNIT_ASSIGNED_CONTEXT ( ( #3239, #11743, #11832 ) ) REPRESENTATION_CONTEXT ( 'NONE', 'WORKASPACE' ) );
#3598 = CARTESIAN_POINT ( 'NONE',  ( 26.39823381822651882, -6.110324093391315436, 7.939653947423658487 ) ) ;
#3599 = ORIENTED_EDGE ( 'NONE', *, *, #10221, .T. ) ;
#3600 = DIRECTION ( 'NONE',  ( -1.000000000000000000, 0.000000000000000000, 0.000000000000000000 ) ) ;
#3601 = ORIENTED_EDGE ( 'NONE', *, *, #4512, .T. ) ;
#3602 = CARTESIAN_POINT ( 'NONE',  ( 26.21417678486618641, -2.370676134166772808, 5.783357778048668685 ) ) ;
#3603 = CARTESIAN_POINT ( 'NONE',  ( -29.25000000000000000, -16.21813761408365195, 13.37255996287876947 ) ) ;
#3604 = DIRECTION ( 'NONE',  ( 0.000000000000000000, -1.000000000000000000, 0.000000000000000000 ) ) ;
#3605 = EDGE_CURVE ( 'NONE', #17262, #225, #7021, .T. ) ;
#3606 = ORIENTED_EDGE ( 'NONE', *, *, #9596, .T. ) ;
#3607 = CARTESIAN_POINT ( 'NONE',  ( 33.83947189604607786, -2.952629194728097595, 5.783357778048663356 ) ) ;
#3608 = DIRECTION ( 'NONE',  ( -0.1196152422706621005, -0.9928203230275509661, -0.000000000000000000 ) ) ;
#3609 = PLANE ( 'NONE',  #13979 ) ;
#3610 = CARTESIAN_POINT ( 'NONE',  ( 32.69811611091622439, -2.216460025892273311, -6.861505862736158257 ) ) ;
#3611 = CARTESIAN_POINT ( 'NONE',  ( 32.04158527077989760, -6.057382223572642665, -4.705209693361168455 ) ) ;
#3612 = DIRECTION ( 'NONE',  ( 1.000000000000000000, 0.000000000000000000, 0.000000000000000000 ) ) ;
#3613 = CARTESIAN_POINT ( 'NONE',  ( 31.66176685062031027, -1.704152250161192539, -6.453230759126468818 ) ) ;
#3614 = CARTESIAN_POINT ( 'NONE',  ( 27.51889869220010354, -3.467423976192371082, -7.939653947423660263 ) ) ;
#3615 = PRODUCT ( 'heat isolation block', 'heat isolation block', '', ( #13914 ) ) ;
#3616 = CYLINDRICAL_SURFACE ( 'NONE', #8624, 5.500000000000000888 ) ;
#3617 = CARTESIAN_POINT ( 'NONE',  ( -4.000000000000000000, 2.309401076758501592, -0.4999999999999963363 ) ) ;
#3618 = DIRECTION ( 'NONE',  ( 0.1196152422706618645, -0.9928203230275510771, 0.000000000000000000 ) ) ;
#3619 = CARTESIAN_POINT ( 'NONE',  ( 31.15208055228630357, -2.102918000029084578, 7.033357778048666020 ) ) ;
#3620 = ORIENTED_EDGE ( 'NONE', *, *, #3254, .F. ) ;
#3621 = ORIENTED_EDGE ( 'NONE', *, *, #17240, .T. ) ;
#3622 = ORIENTED_EDGE ( 'NONE', *, *, #9712, .T. ) ;
#3623 = CARTESIAN_POINT ( 'NONE',  ( 25.71748644841968456, -2.420320648352046078, -5.783357778048663356 ) ) ;
#3624 = CARTESIAN_POINT ( 'NONE',  ( 32.30426898124760982, -6.025734024055190652, 4.705209693361159573 ) ) ;
#3625 = EDGE_LOOP ( 'NONE', ( #1582, #7348, #2283, #14185 ) ) ;
#3626 = PLANE ( 'NONE',  #7195 ) ;
#3627 = EDGE_CURVE ( 'NONE', #17548, #397, #2269, .T. ) ;
#3628 = DIRECTION ( 'NONE',  ( 1.000000000000000000, 0.000000000000000000, 0.000000000000000000 ) ) ;
#3629 = CARTESIAN_POINT ( 'NONE',  ( 27.24868051476284236, -2.235842002054281075, -6.453230759126464378 ) ) ;
#3630 = CARTESIAN_POINT ( 'NONE',  ( 28.71854711534694715, -4.576831098024959132, -3.627061608673664672 ) ) ;
#3631 = FACE_OUTER_BOUND ( 'NONE', #17920, .T. ) ;
#3632 = CARTESIAN_POINT ( 'NONE',  ( -15.92260893619738837, -28.39189527176317540, 6.000000000000000000 ) ) ;
#3633 = CARTESIAN_POINT ( 'NONE',  ( 45.00000000000000711, -19.03270077640483038, -0.5379818257722508434 ) ) ;
#3634 = FACE_BOUND ( 'NONE', #12027, .T. ) ;
#3635 = CARTESIAN_POINT ( 'NONE',  ( 29.70732014299206369, -2.276983097582480742, -7.033357778048658027 ) ) ;
#3636 = EDGE_CURVE ( 'NONE', #7716, #4413, #16915, .T. ) ;
#3637 = ORIENTED_EDGE ( 'NONE', *, *, #17620, .T. ) ;
#3638 = CARTESIAN_POINT ( 'NONE',  ( 27.12505156253147476, -7.276697974355294640, -5.783357778048668685 ) ) ;
#3639 = CARTESIAN_POINT ( 'NONE',  ( 32.82963640218302004, -5.962437625020304388, -4.705209693361169343 ) ) ;
#3640 = VERTEX_POINT ( 'NONE', #3382 ) ;
#3641 = CARTESIAN_POINT ( 'NONE',  ( 0.6666666666666659635, -4.233901974057268980, -3.000726591567087098 ) ) ;
#3642 = CARTESIAN_POINT ( 'NONE',  ( 26.39379627684682106, -4.856917663858078882, 8.283357778048662468 ) ) ;
#3643 = EDGE_LOOP ( 'NONE', ( #3916, #14619, #4515, #16461, #2780 ) ) ;
#3644 = CARTESIAN_POINT ( 'NONE',  ( 4.000000000000000000, 0.1981133338132479993, -1.407451120981426406E-15 ) ) ;
#3645 = CARTESIAN_POINT ( 'NONE',  ( 31.71314141467879111, -4.216041623526076698, -3.627061608673664672 ) ) ;
#3646 = ORIENTED_EDGE ( 'NONE', *, *, #3369, .F. ) ;
#3647 = EDGE_CURVE ( 'NONE', #10267, #11388, #12897, .T. ) ;
#3648 = CARTESIAN_POINT ( 'NONE',  ( 45.00000000000000711, -19.03270077640482683, -10.53798182577225084 ) ) ;
#3649 = LINE ( 'NONE', #8905, #10490 ) ;
#3650 = CARTESIAN_POINT ( 'NONE',  ( -23.00000000000000000, -16.21813761408365195, -13.00000000000000178 ) ) ;
#3651 = CARTESIAN_POINT ( 'NONE',  ( -4.000000000000000888, -1.539600717839008315, -3.000726591567082657 ) ) ;
#3652 = CARTESIAN_POINT ( 'NONE',  ( 32.53688598753899441, -6.297517047505613697, -7.033357778048666908 ) ) ;
#3653 = EDGE_CURVE ( 'NONE', #3230, #10383, #8916, .T. ) ;
#3654 = CARTESIAN_POINT ( 'NONE',  ( 28.25893984004492765, -6.513116296623863377, -4.705209693361168455 ) ) ;
#3655 = CARTESIAN_POINT ( 'NONE',  ( -23.02601376483258022, 3.965314980223224151, 6.000000000000000000 ) ) ;
#3656 = CARTESIAN_POINT ( 'NONE',  ( 0.3198814748697599297, 4.434118497892178823, -0.3507732604232501328 ) ) ;
#3657 = CARTESIAN_POINT ( 'NONE',  ( 27.78220930431293922, -1.782014143258494832, -5.783357778048658027 ) ) ;
#3658 = CARTESIAN_POINT ( 'NONE',  ( 32.54503264317084188, -5.369756224683081669, -3.627061608673667781 ) ) ;
#3659 = CARTESIAN_POINT ( 'NONE',  ( -34.91600907648203389, -11.88801210197604341, -12.00000000000000000 ) ) ;
#3660 = CARTESIAN_POINT ( 'NONE',  ( 30.25524682244395436, -4.391689130744175884, -3.283357778048664688 ) ) ;
#3661 = ORIENTED_EDGE ( 'NONE', *, *, #5483, .T. ) ;
#3662 = CARTESIAN_POINT ( 'NONE',  ( 26.16909369068367752, -6.168712907020688974, 3.640912447338509939 ) ) ;
#3663 = DIRECTION ( 'NONE',  ( -0.1196152422706609625, 0.9928203230275510771, -4.694733121053619507E-17 ) ) ;
#3664 = CARTESIAN_POINT ( 'NONE',  ( 33.44685390376565692, -4.007163506710925027, -7.939653947423662039 ) ) ;
#3665 = CARTESIAN_POINT ( 'NONE',  ( -9.458171371211065548, -3.728626979641334493, -2.666481567098320404 ) ) ;
#3666 = CARTESIAN_POINT ( 'NONE',  ( 29.26075783691881682, -2.330785036554694489, -4.533357778048659803 ) ) ;
#3667 = CARTESIAN_POINT ( 'NONE',  ( -2.804994570502171491, -3.229033611042460006, -3.226374918436839767 ) ) ;
#3668 = ITEM_DEFINED_TRANSFORMATION ( 'NONE', 'NONE', #5638,  #3575 ) ;
#3669 = CARTESIAN_POINT ( 'NONE',  ( -35.19141017012124451, -14.17387298022714148, 11.46934516270795079 ) ) ;
#3670 = CARTESIAN_POINT ( 'NONE',  ( 26.56758885001203652, -2.317900097157796324, -5.783357778048670461 ) ) ;
#3671 = CARTESIAN_POINT ( 'NONE',  ( 28.91547068018125799, -2.672194098943493135, -6.861505862736158257 ) ) ;
#3672 = EDGE_CURVE ( 'NONE', #15335, #14228, #10617, .T. ) ;
#3673 = CARTESIAN_POINT ( 'NONE',  ( 2.500000000000000000, 2.357898499370432166, -2.385244779468109755E-15 ) ) ;
#3674 = CARTESIAN_POINT ( 'NONE',  ( 29.25000000000000000, -16.21813761408365195, -13.37255996287876236 ) ) ;
#3675 = CARTESIAN_POINT ( 'NONE',  ( 25.76326615456878244, -3.051972493152843580, 4.705209693361168455 ) ) ;
#3676 = AXIS2_PLACEMENT_3D ( 'NONE', #13531, #6629, #12155 ) ;
#3677 = VERTEX_POINT ( 'NONE', #2132 ) ;
#3678 = CARTESIAN_POINT ( 'NONE',  ( 31.67382807612511542, -6.101689702897060030, 4.705209693361159573 ) ) ;
#3679 = CARTESIAN_POINT ( 'NONE',  ( 27.30498922523054617, -2.229057914452205136, 6.453230759126474148 ) ) ;
#3680 = CARTESIAN_POINT ( 'NONE',  ( -4.000000000000000000, -2.309401076758508253, -3.133295621305383083 ) ) ;
#3681 = EDGE_CURVE ( 'NONE', #12087, #4193, #15900, .T. ) ;
#3682 = ORIENTED_EDGE ( 'NONE', *, *, #9212, .T. ) ;
#3683 = DIRECTION ( 'NONE',  ( 0.000000000000000000, 0.000000000000000000, -1.000000000000000000 ) ) ;
#3684 = CARTESIAN_POINT ( 'NONE',  ( 1.500000000000000000, 10.05532945112459053, -2.666480854966549519 ) ) ;
#3685 = CARTESIAN_POINT ( 'NONE',  ( 33.15485366002904755, -6.560422763297783177, -5.783357778048663356 ) ) ;
#3686 = CARTESIAN_POINT ( 'NONE',  ( 32.19919549706052209, -6.038393303862174655, -4.705209693361169343 ) ) ;
#3687 = AXIS2_PLACEMENT_3D ( 'NONE', #12340, #16610, #284 ) ;
#3688 = CARTESIAN_POINT ( 'NONE',  ( 32.04158527077989760, -6.057382223572642665, 6.861505862736158257 ) ) ;
#3689 = CARTESIAN_POINT ( 'NONE',  ( 32.54503264317084188, -5.369756224683081669, -3.627061608673667781 ) ) ;
#3690 = CARTESIAN_POINT ( 'NONE',  ( 29.79859849048667897, -1.928627242885762705, 5.783357778048662468 ) ) ;
#3691 = SHAPE_REPRESENTATION_RELATIONSHIP ( 'NONE' , 'NONE' ,  #3339, #5711 ) ;
#3692 = CARTESIAN_POINT ( 'NONE',  ( 28.34209327568754233, -5.876127416962207306, -7.939653947423664704 ) ) ;
#3693 = EDGE_CURVE ( 'NONE', #9123, #3859, #2034, .T. ) ;
#3694 = CARTESIAN_POINT ( 'NONE',  ( -8.968477750016525363, -19.11972035685536042, 16.82776078363834671 ) ) ;
#3695 = CARTESIAN_POINT ( 'NONE',  ( 27.90727577511918867, -2.156494279411373061, 5.783357778048657138 ) ) ;
#3696 = CARTESIAN_POINT ( 'NONE',  ( 28.79925754835455010, -6.020920669644549861, 3.283357778048663800 ) ) ;
#3697 = ORIENTED_EDGE ( 'NONE', *, *, #578, .F. ) ;
#3698 = ORIENTED_EDGE ( 'NONE', *, *, #14726, .F. ) ;
#3699 = ORIENTED_EDGE ( 'NONE', *, *, #13392, .F. ) ;
#3700 = CARTESIAN_POINT ( 'NONE',  ( 32.51858583609114106, -1.611119345748072362, 5.783357778048668685 ) ) ;
#3701 = CARTESIAN_POINT ( 'NONE',  ( 28.49970350196817392, -5.857138497251737519, 3.627061608673662896 ) ) ;
#3702 = VERTEX_POINT ( 'NONE', #7558 ) ;
#3703 = DIRECTION ( 'NONE',  ( -1.000000000000000000, 0.000000000000000000, 0.000000000000000000 ) ) ;
#3704 = AXIS2_PLACEMENT_3D ( 'NONE', #17279, #401, #10071 ) ;
#3705 = FACE_OUTER_BOUND ( 'NONE', #14084, .T. ) ;
#3706 = LINE ( 'NONE', #13320, #13380 ) ;
#3707 = CARTESIAN_POINT ( 'NONE',  ( 30.18087924896149588, -5.654590020340094725, -3.627061608673668225 ) ) ;
#3708 = DIRECTION ( 'NONE',  ( 0.05980762113533059227, -0.4964101615137756496, -0.8660254037844385966 ) ) ;
#3709 = CARTESIAN_POINT ( 'NONE',  ( 31.74131510559286085, -5.666460835049168310, -3.283357778048667797 ) ) ;
#3710 = LINE ( 'NONE', #2006, #2400 ) ;
#3711 = CARTESIAN_POINT ( 'NONE',  ( 27.12922144900085186, -2.887401855662130146, -4.705209693361160461 ) ) ;
#3712 = CARTESIAN_POINT ( 'NONE',  ( 33.86058074732183343, -3.957317592522819005, -3.455209693361164902 ) ) ;
#3713 =( LENGTH_UNIT ( ) NAMED_UNIT ( * ) SI_UNIT ( .MILLI., .METRE. ) );
#3714 = EDGE_LOOP ( 'NONE', ( #7431, #1956, #48, #9036, #10400, #4315 ) ) ;
#3715 = CIRCLE ( 'NONE', #6012, 0.9000000000000003553 ) ;
#3716 = CARTESIAN_POINT ( 'NONE',  ( 32.80318959510331212, -2.203800746085299522, -4.705209693361160461 ) ) ;
#3717 = CARTESIAN_POINT ( 'NONE',  ( 31.43723430067123914, -2.368371383576012956, -6.861505862736158257 ) ) ;
#3718 = ORIENTED_EDGE ( 'NONE', *, *, #7188, .F. ) ;
#3719 = CARTESIAN_POINT ( 'NONE',  ( 31.88017671309158274, -6.376637546091784792, 7.033357778048657138 ) ) ;
#3720 = VECTOR ( 'NONE', #16876, 1000.000000000000000 ) ;
#3721 = CARTESIAN_POINT ( 'NONE',  ( 26.30185955129047315, -7.986322017489088765, 4.917936583846921117 ) ) ;
#3722 = AXIS2_PLACEMENT_3D ( 'NONE', #14383, #7673, #505 ) ;
#3723 = ORIENTED_EDGE ( 'NONE', *, *, #11795, .T. ) ;
#3724 = CARTESIAN_POINT ( 'NONE',  ( 29.38468146192651886, -6.677295441714964142, -7.033357778048666908 ) ) ;
#3725 = CARTESIAN_POINT ( 'NONE',  ( 31.39792096211754924, -4.254019462947003838, -7.939653947423662039 ) ) ;
#3726 = CARTESIAN_POINT ( 'NONE',  ( 21.42601376483257880, 2.765314980223224417, -12.00000000000000000 ) ) ;
#3727 = LINE ( 'NONE', #11974, #17491 ) ;
#3728 = CARTESIAN_POINT ( 'NONE',  ( 28.82057243903374655, -7.082618055128190093, -5.783357778048668685 ) ) ;
#3729 = AXIS2_PLACEMENT_3D ( 'NONE', #6931, #12464, #12199 ) ;
#3730 = CARTESIAN_POINT ( 'NONE',  ( 0.6641139335921072417, -4.471067008846246971, -3.302142222889021372 ) ) ;
#3731 = UNCERTAINTY_MEASURE_WITH_UNIT (LENGTH_MEASURE( 1.000000000000000082E-05 ), #3713, 'distance_accuracy_value', 'NONE');
#3732 = CARTESIAN_POINT ( 'NONE',  ( 32.38298487551052318, -4.135338714860305132, -8.283357778048662468 ) ) ;
#3733 = ORIENTED_EDGE ( 'NONE', *, *, #443, .F. ) ;
#3734 = CARTESIAN_POINT ( 'NONE',  ( 33.30246708102489350, -5.905470865888903020, -4.705209693361168455 ) ) ;
#3735 = DIRECTION ( 'NONE',  ( 0.5661261679878573094, 0.8243186046180107640, 0.000000000000000000 ) ) ;
#3736 = CARTESIAN_POINT ( 'NONE',  ( 3.248936832696173393, -28.97437970944926633, -17.00000000000000000 ) ) ;
#3737 = FACE_OUTER_BOUND ( 'NONE', #15811, .T. ) ;
#3738 = CARTESIAN_POINT ( 'NONE',  ( 28.55151181693415907, -2.416235175459247486, -4.533357778048659803 ) ) ;
#3739 = EDGE_CURVE ( 'NONE', #12847, #11807, #4647, .T. ) ;
#3740 = CARTESIAN_POINT ( 'NONE',  ( 30.64918316926811315, -2.463315982128351678, -6.861505862736159145 ) ) ;
#3741 = AXIS2_PLACEMENT_3D ( 'NONE', #845, #6284, #14960 ) ;
#3742 = EDGE_LOOP ( 'NONE', ( #11340, #14046 ) ) ;
#3743 = EDGE_CURVE ( 'NONE', #15480, #60, #7653, .T. ) ;
#3744 = ADVANCED_FACE ( 'NONE', ( #9004 ), #1947, .T. ) ;
#3745 = ORIENTED_EDGE ( 'NONE', *, *, #3490, .T. ) ;
#3746 = DIRECTION ( 'NONE',  ( 0.05980762113533044655, -0.4964101615137759826, 0.8660254037844383745 ) ) ;
#3747 = DIRECTION ( 'NONE',  ( 0.000000000000000000, 0.000000000000000000, -1.000000000000000000 ) ) ;
#3748 = ORIENTED_EDGE ( 'NONE', *, *, #9942, .F. ) ;
#3749 =( NAMED_UNIT ( * ) SI_UNIT ( $, .STERADIAN. ) SOLID_ANGLE_UNIT ( ) );
#3750 = AXIS2_PLACEMENT_3D ( 'NONE', #10192, #1962, #10363 ) ;
#3751 = PRODUCT_DEFINITION_SHAPE ( 'NONE', 'NONE',  #17972 ) ;
#3752 = CARTESIAN_POINT ( 'NONE',  ( -1.500000000000000000, -11.00000000000000000, -2.000000000000000000 ) ) ;
#3753 = DIRECTION ( 'NONE',  ( 0.9928203230275510771, 0.1196152422706614621, -0.000000000000000000 ) ) ;
#3754 = ORIENTED_EDGE ( 'NONE', *, *, #2082, .F. ) ;
#3755 = AXIS2_PLACEMENT_3D ( 'NONE', #10039, #370, #1912 ) ;
#3756 = ORIENTED_EDGE ( 'NONE', *, *, #10540, .F. ) ;
#3757 = CARTESIAN_POINT ( 'NONE',  ( 33.60446413004628141, -3.988174587000466342, -3.627061608673664672 ) ) ;
#3758 = CARTESIAN_POINT ( 'NONE',  ( 7.374038404635976818, 5.989453865500072638, -2.000000000000000000 ) ) ;
#3759 = B_SPLINE_CURVE_WITH_KNOTS ( 'NONE', 3,
 ( #17890, #13856, #2798, #10934 ),
 .UNSPECIFIED., .F., .F.,
 ( 4, 4 ),
 ( 0.007932485430080135971, 0.009354825709699443950 ),
 .UNSPECIFIED. ) ;
#3760 = FACE_OUTER_BOUND ( 'NONE', #9580, .T. ) ;
#3761 = DIRECTION ( 'NONE',  ( 0.000000000000000000, 0.000000000000000000, 1.000000000000000000 ) ) ;
#3762 = CARTESIAN_POINT ( 'NONE',  ( 31.45915434921569798, -2.992700983430681028, -7.939653947423660263 ) ) ;
#3763 = ADVANCED_FACE ( 'NONE', ( #13176 ), #10173, .T. ) ;
#3764 = CARTESIAN_POINT ( 'NONE',  ( 33.42946061375642586, -6.517141185936593750, -5.783357778048668685 ) ) ;
#3765 = CARTESIAN_POINT ( 'NONE',  ( 25.76872643656706074, -21.83605427490913797, -14.29305147543152366 ) ) ;
#3766 = CARTESIAN_POINT ( 'NONE',  ( 30.96820195323705605, -2.125071739898741097, 4.533357778048667797 ) ) ;
#3767 = ORIENTED_EDGE ( 'NONE', *, *, #5434, .T. ) ;
#3768 = EDGE_LOOP ( 'NONE', ( #387, #8537 ) ) ;
#3769 = EDGE_CURVE ( 'NONE', #15072, #12450, #6094, .T. ) ;
#3770 = CARTESIAN_POINT ( 'NONE',  ( 30.81132015408399027, -5.578634341498224458, 7.939653947423658487 ) ) ;
#3771 = CARTESIAN_POINT ( 'NONE',  ( -25.01528890617809253, -10.29849948291661121, 14.47305271942837557 ) ) ;
#3772 = DIRECTION ( 'NONE',  ( -1.000000000000000000, 0.000000000000000000, 0.000000000000000000 ) ) ;
#3773 = VERTEX_POINT ( 'NONE', #5910 ) ;
#3774 = CARTESIAN_POINT ( 'NONE',  ( 33.18300801526289234, -6.557030719496743210, -6.453230759126470595 ) ) ;
#3775 = CARTESIAN_POINT ( 'NONE',  ( 1.500000000000000000, 10.39230484541326227, -3.000000000000000000 ) ) ;
#3776 = EDGE_CURVE ( 'NONE', #16386, #15079, #7466, .T. ) ;
#3777 = DIRECTION ( 'NONE',  ( -0.05980762113533043267, 0.4964101615137759826, -0.8660254037844384856 ) ) ;
#3778 = CARTESIAN_POINT ( 'NONE',  ( 30.29464937815318493, -4.386941900920275472, -7.939653947423662039 ) ) ;
#3779 = CARTESIAN_POINT ( 'NONE',  ( 4.211140560182196957, 2.431303136016537803, -3.445885042887434579 ) ) ;
#3780 = CARTESIAN_POINT ( 'NONE',  ( 39.55500000000002103, 0.000000000000000000, 0.000000000000000000 ) ) ;
#3781 = CARTESIAN_POINT ( 'NONE',  ( 27.62849893492243325, -6.589071975465733644, 6.861505862736158257 ) ) ;
#3782 = VECTOR ( 'NONE', #6710, 1000.000000000000227 ) ;
#3783 = EDGE_CURVE ( 'NONE', #13090, #3230, #13534, .T. ) ;
#3784 =( GEOMETRIC_REPRESENTATION_CONTEXT ( 3 ) GLOBAL_UNCERTAINTY_ASSIGNED_CONTEXT ( ( #4445 ) ) GLOBAL_UNIT_ASSIGNED_CONTEXT ( ( #13509, #2103, #811 ) ) REPRESENTATION_CONTEXT ( 'NONE', 'WORKASPACE' ) );
#3785 = CARTESIAN_POINT ( 'NONE',  ( 10.50000000000000000, 1.285879139104720831E-15, -3.000000000000002665 ) ) ;
#3786 = CARTESIAN_POINT ( 'NONE',  ( 27.95866967485789090, -6.122194908100387245, -3.283357778048667797 ) ) ;
#3787 = CARTESIAN_POINT ( 'NONE',  ( 32.49625839967270480, -6.639770485940693412, -5.113484796970860558 ) ) ;
#3788 = CARTESIAN_POINT ( 'NONE',  ( 28.63031693179632242, -2.406740715396564756, 7.033357778048666020 ) ) ;
#3789 = B_SPLINE_CURVE_WITH_KNOTS ( 'NONE', 3,
 ( #2183, #4784, #13043, #14413 ),
 .UNSPECIFIED., .F., .F.,
 ( 4, 4 ),
 ( 0.000000000000000000, 0.0006487028241592422868 ),
 .UNSPECIFIED. ) ;
#3790 = AXIS2_PLACEMENT_3D ( 'NONE', #15708, #11701, #3558 ) ;
#3791 = ORIENTED_EDGE ( 'NONE', *, *, #5183, .T. ) ;
#3792 = CIRCLE ( 'NONE', #16255, 2.540000000000001368 ) ;
#3793 = ORIENTED_EDGE ( 'NONE', *, *, #2471, .T. ) ;
#3794 = ORIENTED_EDGE ( 'NONE', *, *, #13595, .F. ) ;
#3795 = CARTESIAN_POINT ( 'NONE',  ( 32.75517961154501023, -5.344437665069116328, 3.627061608673662896 ) ) ;
#3796 =( REPRESENTATION_RELATIONSHIP ('NONE','NONE', #3227, #3339 ) REPRESENTATION_RELATIONSHIP_WITH_TRANSFORMATION ( #14572 )SHAPE_REPRESENTATION_RELATIONSHIP( ) );
#3797 = CARTESIAN_POINT ( 'NONE',  ( 31.44176105920648112, -5.502678662656354192, 7.939653947423658487 ) ) ;
#3798 = VERTEX_POINT ( 'NONE', #11623 ) ;
#3799 = CARTESIAN_POINT ( 'NONE',  ( 30.68374079916737429, -6.858143062403621926, 6.453230759126467042 ) ) ;
#3800 = CIRCLE ( 'NONE', #3510, 6.249999999999998224 ) ;
#3801 = CYLINDRICAL_SURFACE ( 'NONE', #13881, 13.00000000000000178 ) ;
#3802 = ADVANCED_FACE ( 'NONE', ( #15624 ), #14272, .T. ) ;
#3803 = COLOUR_RGB ( '', 0.66274510, 0.83137255, 0.94901961) ;
#3804 = CARTESIAN_POINT ( 'NONE',  ( 29.62480591732145996, -4.467644809586046151, -3.283357778048664688 ) ) ;
#3805 = CARTESIAN_POINT ( 'NONE',  ( 29.14753769709988518, -3.271205139184214516, -3.627061608673662008 ) ) ;
#3806 = CARTESIAN_POINT ( 'NONE',  ( 38.69874410340102600, -1.484456793942448449, -2.033357778048666464 ) ) ;
#3807 = VERTEX_POINT ( 'NONE', #7734 ) ;
#3808 = CARTESIAN_POINT ( 'NONE',  ( 32.55182397003001427, -2.661183353387966299, -3.283357778048662023 ) ) ;
#3809 = FACE_OUTER_BOUND ( 'NONE', #5634, .T. ) ;
#3810 = CARTESIAN_POINT ( 'NONE',  ( 26.85044460880409645, -7.319979551716484067, -5.783357778048668685 ) ) ;
#3811 = VECTOR ( 'NONE', #15051, 999.9999999999998863 ) ;
#3812 = CARTESIAN_POINT ( 'NONE',  ( -45.50000000000000000, -19.03270077640483038, 2.787981825772258837 ) ) ;
#3813 = AXIS2_PLACEMENT_3D ( 'NONE', #3959, #6770, #59 ) ;
#3814 = CARTESIAN_POINT ( 'NONE',  ( 30.40841950734487753, -3.119293781500474427, -3.627061608673662008 ) ) ;
#3815 = DIRECTION ( 'NONE',  ( -1.000000000000000000, 0.000000000000000000, 0.000000000000000000 ) ) ;
#3816 = EDGE_LOOP ( 'NONE', ( #4598, #10832, #4008, #10200 ) ) ;
#3817 = CARTESIAN_POINT ( 'NONE',  ( 31.08763465596552322, -1.773323841400983758, 6.453230759126472371 ) ) ;
#3818 = CARTESIAN_POINT ( 'NONE',  ( 46.86575133767496482, -2.390451368237048513, -5.783357778048662468 ) ) ;
#3819 = ORIENTED_EDGE ( 'NONE', *, *, #4860, .T. ) ;
#3820 = CARTESIAN_POINT ( 'NONE',  ( 32.97402322492378346, -4.064130265842336165, 7.939653947423662039 ) ) ;
#3821 = VECTOR ( 'NONE', #4440, 1000.000000000000114 ) ;
#3822 = CARTESIAN_POINT ( 'NONE',  ( 27.73357241910951743, -6.576412695658750529, -6.861505862736166250 ) ) ;
#3823 = EDGE_CURVE ( 'NONE', #2767, #7401, #507, .T. ) ;
#3824 = DIRECTION ( 'NONE',  ( -0.1196152422706598106, 0.9928203230275514102, 0.000000000000000000 ) ) ;
#3825 = B_SPLINE_CURVE_WITH_KNOTS ( 'NONE', 3,
 ( #5439, #383, #15601, #6070, #7183, #10146, #15697, #11599, #17165, #10485, #4532, #15512, #3009, #11412, #14342, #5798, #3177, #3093 ),
 .UNSPECIFIED., .F., .F.,
 ( 4, 2, 2, 2, 2, 2, 2, 2, 4 ),
 ( 0.000000000000000000, 0.0005710890023745246154, 0.001142178004749049231, 0.001713267007123573955, 0.002284356009498098462, 0.002855445011872622969, 0.003426534014247147909, 0.003997623016621672416, 0.004568712018996196923 ),
 .UNSPECIFIED. ) ;
#3826 = CARTESIAN_POINT ( 'NONE',  ( 28.75424055680402802, -6.753251120556833520, -7.033357778048666908 ) ) ;
#3827 = ADVANCED_FACE ( 'NONE', ( #3098 ), #3282, .F. ) ;
#3828 = CARTESIAN_POINT ( 'NONE',  ( 25.87953856062030766, -3.765371892057810754, 7.615734152686682634 ) ) ;
#3829 = CIRCLE ( 'NONE', #11026, 2.041999999999999815 ) ;
#3830 = AXIS2_PLACEMENT_3D ( 'NONE', #6269, #7906, #11885 ) ;
#3831 = FACE_OUTER_BOUND ( 'NONE', #9072, .T. ) ;
#3832 = CARTESIAN_POINT ( 'NONE',  ( 32.92339180097568629, -5.524043937428110063, -3.283357778048667797 ) ) ;
#3833 = CARTESIAN_POINT ( 'NONE',  ( 33.14902674121363901, -1.535163666906202318, -5.783357778048658027 ) ) ;
#3834 = AXIS2_PLACEMENT_3D ( 'NONE', #3063, #158, #5491 ) ;
#3835 = CARTESIAN_POINT ( 'NONE',  ( 25.71748644841968456, -2.420320648352051851, -5.783357778048663356 ) ) ;
#3836 = CARTESIAN_POINT ( 'NONE',  ( 1.654252653721902444, 3.663718938583013340, -0.01223254789873544877 ) ) ;
#3837 = FACE_OUTER_BOUND ( 'NONE', #14362, .T. ) ;
#3838 = DIRECTION ( 'NONE',  ( 0.000000000000000000, 0.000000000000000000, 1.000000000000000000 ) ) ;
#3839 = CARTESIAN_POINT ( 'NONE',  ( 32.77257290155422709, -2.834459985843462260, -3.627061608673662896 ) ) ;
#3840 = CIRCLE ( 'NONE', #8463, 0.9000000000000011324 ) ;
#3841 = AXIS2_PLACEMENT_3D ( 'NONE', #17376, #9177, #1107 ) ;
#3842 = CARTESIAN_POINT ( 'NONE',  ( -8.632250723006720250, -18.84644399697197770, 13.00000000000000178 ) ) ;
#3843 = CYLINDRICAL_SURFACE ( 'NONE', #5502, 2.499999999999999112 ) ;
#3844 = ADVANCED_FACE ( 'NONE', ( #8621 ), #16981, .T. ) ;
#3845 = VERTEX_POINT ( 'NONE', #1745 ) ;
#3846 =( NAMED_UNIT ( * ) PLANE_ANGLE_UNIT ( ) SI_UNIT ( $, .RADIAN. ) );
#3847 = ADVANCED_FACE ( 'NONE', ( #12697, #386 ), #15605, .F. ) ;
#3848 = VECTOR ( 'NONE', #1772, 1000.000000000000000 ) ;
#3849 = DIRECTION ( 'NONE',  ( -0.9979201627913402151, 0.06446199418653550395, 5.311609029246448998E-22 ) ) ;
#3850 = PLANE ( 'NONE',  #12213 ) ;
#3851 = AXIS2_PLACEMENT_3D ( 'NONE', #17013, #7216, #8477 ) ;
#3852 = CARTESIAN_POINT ( 'NONE',  ( 25.37303892199676270, -2.799178389412888546, -7.033357778048658027 ) ) ;
#3853 = CYLINDRICAL_SURFACE ( 'NONE', #5749, 95.00000000000000000 ) ;
#3854 = DIRECTION ( 'NONE',  ( -0.000000000000000000, -0.000000000000000000, -1.000000000000000000 ) ) ;
#3855 = CARTESIAN_POINT ( 'NONE',  ( 28.54354359905709870, -7.105797696961086096, -5.783357778048669573 ) ) ;
#3856 = CARTESIAN_POINT ( 'NONE',  ( 35.74085044863416982, -23.57886868891565513, 11.27079897466147251 ) ) ;
#3857 = AXIS2_PLACEMENT_3D ( 'NONE', #11830, #606, #13117 ) ;
#3858 = CARTESIAN_POINT ( 'NONE',  ( 32.43181250335191379, -6.310176327312596811, 7.033357778048657138 ) ) ;
#3859 = VERTEX_POINT ( 'NONE', #14345 ) ;
#3860 = ORIENTED_EDGE ( 'NONE', *, *, #2101, .T. ) ;
#3861 = CARTESIAN_POINT ( 'NONE',  ( 29.52399153675929355, -1.971908820246954130, 5.783357778048668685 ) ) ;
#3862 =( NAMED_UNIT ( * ) SI_UNIT ( $, .STERADIAN. ) SOLID_ANGLE_UNIT ( ) );
#3863 = CARTESIAN_POINT ( 'NONE',  ( 28.45891156537951971, -2.090033060632186412, 5.783357778048657138 ) ) ;
#3864 = ORIENTED_EDGE ( 'NONE', *, *, #1850, .F. ) ;
#3865 = DIRECTION ( 'NONE',  ( 0.9928203230275512992, 0.1196152422706610180, 4.006172263299093133E-17 ) ) ;
#3866 = EDGE_CURVE ( 'NONE', #3798, #475, #10324, .T. ) ;
#3867 = ORIENTED_EDGE ( 'NONE', *, *, #13954, .F. ) ;
#3868 = CARTESIAN_POINT ( 'NONE',  ( -3.538288549924106796, -15.34800872113743431, 13.00000000000000178 ) ) ;
#3869 = CARTESIAN_POINT ( 'NONE',  ( 30.92509028327567933, -4.310986222078405206, -7.939653947423662039 ) ) ;
#3870 = CARTESIAN_POINT ( 'NONE',  ( 23.00000000000000000, -16.21813761408365195, 13.00000000000000178 ) ) ;
#3871 = VECTOR ( 'NONE', #5874, 1000.000000000000114 ) ;
#3872 = LINE ( 'NONE', #3952, #6363 ) ;
#3873 = DIRECTION ( 'NONE',  ( 0.000000000000000000, 0.000000000000000000, -1.000000000000000000 ) ) ;
#3874 = CARTESIAN_POINT ( 'NONE',  ( 25.62757597683262034, -3.695291012717980994, 3.627061608673666893 ) ) ;
#3875 = EDGE_CURVE ( 'NONE', #7467, #14045, #14107, .T. ) ;
#3876 = EDGE_LOOP ( 'NONE', ( #12501, #917, #4888, #3375 ) ) ;
#3877 = DIRECTION ( 'NONE',  ( 0.000000000000000000, 0.000000000000000000, -1.000000000000000000 ) ) ;
#3878 = CARTESIAN_POINT ( 'NONE',  ( 32.81641299864316608, -4.083119185552795294, 3.627061608673664228 ) ) ;
#3879 = CARTESIAN_POINT ( 'NONE',  ( 27.10304229683147526, -4.771467524953526329, 8.283357778048662468 ) ) ;
#3880 = ORIENTED_EDGE ( 'NONE', *, *, #1366, .F. ) ;
#3881 = ORIENTED_EDGE ( 'NONE', *, *, #431, .F. ) ;
#3882 = ORIENTED_EDGE ( 'NONE', *, *, #17864, .F. ) ;
#3883 = CARTESIAN_POINT ( 'NONE',  ( 30.45225960443380231, -4.367952981209816343, 7.939653947423662039 ) ) ;
#3884 = DIRECTION ( 'NONE',  ( -0.1196152422706610735, 0.9928203230275511881, 0.000000000000000000 ) ) ;
#3885 = CARTESIAN_POINT ( 'NONE',  ( 31.03886041246737548, -3.043338102658604161, 7.939653947423662927 ) ) ;
#3886 = DIRECTION ( 'NONE',  ( -0.1196152422706614343, 0.9928203230275510771, 0.000000000000000000 ) ) ;
#3887 = DIRECTION ( 'NONE',  ( 0.000000000000000000, 0.000000000000000000, 1.000000000000000000 ) ) ;
#3888 = DIRECTION ( 'NONE',  ( -0.000000000000000000, -0.000000000000000000, -1.000000000000000000 ) ) ;
#3889 = CARTESIAN_POINT ( 'NONE',  ( 30.19827253897071273, -3.144612341114420673, -7.939653947423660263 ) ) ;
#3890 = CARTESIAN_POINT ( 'NONE',  ( 26.18940075748478691, -6.337263906362392341, -7.823530922983556124 ) ) ;
#3891 = DIRECTION ( 'NONE',  ( -1.224646799147353207E-16, 1.000000000000000000, 0.000000000000000000 ) ) ;
#3892 = CARTESIAN_POINT ( 'NONE',  ( 0.000000000000000000, 0.000000000000000000, 0.000000000000000000 ) ) ;
#3893 = CARTESIAN_POINT ( 'NONE',  ( 21.42418217458643070, -10.16661967303011771, -15.24537580551290183 ) ) ;
#3894 = CARTESIAN_POINT ( 'NONE',  ( 23.00000000000000000, -16.21813761408365195, 0.000000000000000000 ) ) ;
#3895 = SURFACE_STYLE_FILL_AREA ( #12319 ) ;
#3896 = CARTESIAN_POINT ( 'NONE',  ( 30.17635249042624679, -2.520282741259753045, -6.861505862736158257 ) ) ;
#3897 = CARTESIAN_POINT ( 'NONE',  ( 30.30787278169304244, -6.266260340387784566, -4.705209693361169343 ) ) ;
#3898 = ORIENTED_EDGE ( 'NONE', *, *, #4866, .F. ) ;
#3899 = AXIS2_PLACEMENT_3D ( 'NONE', #17688, #5212, #6015 ) ;
#3900 =( BOUNDED_CURVE ( )  B_SPLINE_CURVE ( 2, ( #11738, #10470, #16032, #14483, #16119, #10287, #966, #3679, #9125 ),
 .UNSPECIFIED., .F., .T. ) 
 B_SPLINE_CURVE_WITH_KNOTS ( ( 3, 2, 2, 2, 3 ),
 ( 0.6730769230769231282, 0.6794871794871795156, 0.6923076923076922906, 0.7051282051282051766, 0.7115384615384615641 ),
 .UNSPECIFIED. ) 
 CURVE ( )  GEOMETRIC_REPRESENTATION_ITEM ( )  RATIONAL_B_SPLINE_CURVE ( ( 0.9330127018922192983, 0.9330127018922198534, 1.000000000000000000, 0.8660254037844387076, 1.000000000000000000, 0.8660254037844387076, 1.000000000000000000, 0.9330127018922194093, 0.9330127018922194093 ) ) 
 REPRESENTATION_ITEM ( '' )  );
#3901 = LINE ( 'NONE', #12237, #1417 ) ;
#3902 = EDGE_CURVE ( 'NONE', #8657, #12849, #5103, .T. ) ;
#3903 = CARTESIAN_POINT ( 'NONE',  ( 26.86291784143654127, -6.981118157082444320, 4.533357778048659803 ) ) ;
#3904 = ORIENTED_EDGE ( 'NONE', *, *, #3183, .T. ) ;
#3905 = ORIENTED_EDGE ( 'NONE', *, *, #10233, .F. ) ;
#3906 = ORIENTED_EDGE ( 'NONE', *, *, #17037, .T. ) ;
#3907 = CARTESIAN_POINT ( 'NONE',  ( 31.88814493096864311, -1.687075024589942407, 5.783357778048668685 ) ) ;
#3908 = CARTESIAN_POINT ( 'NONE',  ( 26.97161122272022382, -2.906390775372597712, -4.705209693361161349 ) ) ;
#3909 = LINE ( 'NONE', #6883, #17696 ) ;
#3910 = EDGE_CURVE ( 'NONE', #5051, #8513, #794, .T. ) ;
#3911 = CARTESIAN_POINT ( 'NONE',  ( 0.000000000000000000, 0.000000000000000000, -8.722503561260788629 ) ) ;
#3912 = CARTESIAN_POINT ( 'NONE',  ( 28.48022645605872327, -3.151730446115816875, -8.283357778048660691 ) ) ;
#3913 = CARTESIAN_POINT ( 'NONE',  ( 25.76466184735054910, -2.811881907026620553, 5.318565573966401061 ) ) ;
#3914 = DIRECTION ( 'NONE',  ( -0.000000000000000000, -0.000000000000000000, 1.000000000000000000 ) ) ;
#3915 = CARTESIAN_POINT ( 'NONE',  ( 30.17644170758179101, -4.401183590806859947, -3.283357778048664688 ) ) ;
#3916 = ORIENTED_EDGE ( 'NONE', *, *, #4860, .F. ) ;
#3917 = CARTESIAN_POINT ( 'NONE',  ( 33.17547354829333273, -5.293800545841212291, -3.627061608673667781 ) ) ;
#3918 = CARTESIAN_POINT ( 'NONE',  ( 26.17715024865825768, -6.235583268514400146, -3.900143082538624739 ) ) ;
#3919 = CARTESIAN_POINT ( 'NONE',  ( 32.14656953781143756, -4.163822094218565972, -3.283357778048664688 ) ) ;
#3920 = CYLINDRICAL_SURFACE ( 'NONE', #14730, 2.499999999999999112 ) ;
#3921 = CARTESIAN_POINT ( 'NONE',  ( 2.500000000000000000, 0.000000000000000000, 0.000000000000000000 ) ) ;
#3922 = ADVANCED_FACE ( 'NONE', ( #3592 ), #9282, .F. ) ;
#3923 = CARTESIAN_POINT ( 'NONE',  ( 32.64557936882268052, -2.222789665795767089, -4.705209693361161349 ) ) ;
#3924 = EDGE_CURVE ( 'NONE', #6169, #8696, #9457, .T. ) ;
#3925 = ORIENTED_EDGE ( 'NONE', *, *, #13098, .F. ) ;
#3926 = CARTESIAN_POINT ( 'NONE',  ( -15.92260893619738837, -28.39189527176317540, 16.15082599432113142 ) ) ;
#3927 = EDGE_LOOP ( 'NONE', ( #8850, #16570, #12153, #14710, #7826, #12028 ) ) ;
#3928 = STYLED_ITEM ( 'NONE', ( #54 ), #7249 ) ;
#3929 = CARTESIAN_POINT ( 'NONE',  ( -27.11337801594864061, -11.49512195020015604, -13.95421129451976050 ) ) ;
#3930 = ORIENTED_EDGE ( 'NONE', *, *, #7071, .T. ) ;
#3931 = PRESENTATION_STYLE_ASSIGNMENT (( #16368 ) ) ;
#3932 = CARTESIAN_POINT ( 'NONE',  ( 31.04338717100262102, -6.177645381738930297, -6.861505862736167138 ) ) ;
#3933 = LINE ( 'NONE', #14984, #1225 ) ;
#3934 = CARTESIAN_POINT ( 'NONE',  ( 32.97402322492378346, -4.064130265842336165, -3.627061608673664672 ) ) ;
#3935 = DIRECTION ( 'NONE',  ( -1.000000000000000000, 0.000000000000000000, 0.000000000000000000 ) ) ;
#3936 = DIRECTION ( 'NONE',  ( 0.9928203230275512992, 0.1196152422706610180, 4.006172263299093133E-17 ) ) ;
#3937 = CARTESIAN_POINT ( 'NONE',  ( 27.65911562847151117, -5.958412735707574015, -3.627061608673668225 ) ) ;
#3938 = EDGE_CURVE ( 'NONE', #16041, #16203, #17217, .T. ) ;
#3939 = CARTESIAN_POINT ( 'NONE',  ( 28.91480295676398171, -18.24795679052564168, -13.46730161501605316 ) ) ;
#3940 = CARTESIAN_POINT ( 'NONE',  ( 33.16732689266149237, -6.221561368663743430, 4.533357778048659803 ) ) ;
#3941 = ORIENTED_EDGE ( 'NONE', *, *, #11895, .T. ) ;
#3942 = EDGE_CURVE ( 'NONE', #3060, #2784, #16108, .T. ) ;
#3943 = CARTESIAN_POINT ( 'NONE',  ( 29.13014440709066832, -5.781182818409868140, 3.627061608673662896 ) ) ;
#3944 = DIRECTION ( 'NONE',  ( -0.000000000000000000, -0.000000000000000000, -1.000000000000000000 ) ) ;
#3945 = ADVANCED_FACE ( 'NONE', ( #12178 ), #16019, .T. ) ;
#3946 = VERTEX_POINT ( 'NONE', #2412 ) ;
#3947 = CARTESIAN_POINT ( 'NONE',  ( 8.968924017731504605, -19.12031538047531853, 16.82773324567541451 ) ) ;
#3948 = VERTEX_POINT ( 'NONE', #17668 ) ;
#3949 = CARTESIAN_POINT ( 'NONE',  ( 33.32864623319426300, -4.021405196597508613, -3.283357778048664688 ) ) ;
#3950 = CARTESIAN_POINT ( 'NONE',  ( 31.02146712245815507, -5.553315781884258229, -7.939653947423664704 ) ) ;
#3951 = CARTESIAN_POINT ( 'NONE',  ( -4.000000000000000000, -1.560351142792947732, -0.2242961665059824417 ) ) ;
#3952 = CARTESIAN_POINT ( 'NONE',  ( 39.19942832275109623, -5.640193629429882449, -1.783357778048662690 ) ) ;
#3953 = CARTESIAN_POINT ( 'NONE',  ( 1.296864337298335788E-21, -1.182044466681725685E-21, -6.899999999999998579 ) ) ;
#3954 = CARTESIAN_POINT ( 'NONE',  ( 33.00219691583784964, -5.514549477365426888, 8.283357778048660691 ) ) ;
#3955 = VERTEX_POINT ( 'NONE', #14988 ) ;
#3956 = CARTESIAN_POINT ( 'NONE',  ( 30.67110321781257909, -3.087645581983020637, 3.627061608673666893 ) ) ;
#3957 = CARTESIAN_POINT ( 'NONE',  ( 1.500000000000000222, 9.380831519646861238, -2.000000000000000000 ) ) ;
#3958 = FACE_OUTER_BOUND ( 'NONE', #13769, .T. ) ;
#3959 = CARTESIAN_POINT ( 'NONE',  ( -45.00000000000000711, -19.03270077640483038, 5.537981825772250843 ) ) ;
#3960 = ORIENTED_EDGE ( 'NONE', *, *, #16801, .T. ) ;
#3961 = CARTESIAN_POINT ( 'NONE',  ( 29.12189622942009493, -1.620608325512071568, 5.783357778048668685 ) ) ;
#3962 = EDGE_CURVE ( 'NONE', #8890, #7124, #13810, .T. ) ;
#3963 = ORIENTED_EDGE ( 'NONE', *, *, #1484, .T. ) ;
#3964 = ORIENTED_EDGE ( 'NONE', *, *, #16776, .T. ) ;
#3965 = ORIENTED_EDGE ( 'NONE', *, *, #4119, .T. ) ;
#3966 = CARTESIAN_POINT ( 'NONE',  ( 30.01874226414561875, -2.539271660970221944, 4.705209693361167567 ) ) ;
#3967 = CARTESIAN_POINT ( 'NONE',  ( 38.74759774169763915, -1.889947633019406270, 3.759232513472238413 ) ) ;
#3968 = ORIENTED_EDGE ( 'NONE', *, *, #5286, .T. ) ;
#3969 = CARTESIAN_POINT ( 'NONE',  ( 28.91547068018125799, -2.672194098943493135, 4.705209693361168455 ) ) ;
#3970 = ADVANCED_FACE ( 'NONE', ( #6563 ), #7933, .F. ) ;
#3971 = VECTOR ( 'NONE', #16088, 1000.000000000000000 ) ;
#3972 =( NAMED_UNIT ( * ) SI_UNIT ( $, .STERADIAN. ) SOLID_ANGLE_UNIT ( ) );
#3973 = FACE_OUTER_BOUND ( 'NONE', #14850, .T. ) ;
#3974 = CARTESIAN_POINT ( 'NONE',  ( 25.76326615456878244, -3.051972493152843580, -6.861505862736158257 ) ) ;
#3975 = CARTESIAN_POINT ( 'NONE',  ( 13.00000000000000178, 0.000000000000000000, -12.00000000000000000 ) ) ;
#3976 = CARTESIAN_POINT ( 'NONE',  ( 26.31556265977298992, -7.384422263489805793, -5.783357778048663356 ) ) ;
#3977 = CARTESIAN_POINT ( 'NONE',  ( 26.01652455409633902, -4.902371455920928156, -5.783357778048663356 ) ) ;
#3978 = VECTOR ( 'NONE', #14739, 1000.000000000000227 ) ;
#3979 = CARTESIAN_POINT ( 'NONE',  ( 22.62608969754382215, -9.966271075498049470, -15.00374444583767897 ) ) ;
#3980 =( LENGTH_UNIT ( ) NAMED_UNIT ( * ) SI_UNIT ( .MILLI., .METRE. ) );
#3981 = CARTESIAN_POINT ( 'NONE',  ( 31.41531425212677675, -1.744041783721344219, -5.783357778048658027 ) ) ;
#3982 = CARTESIAN_POINT ( 'NONE',  ( 27.75966235412334981, -2.811446176820259879, -4.705209693361160461 ) ) ;
#3983 = CARTESIAN_POINT ( 'NONE',  ( 31.94462260941237020, -6.706231704719880504, 6.453230759126467042 ) ) ;
#3984 = ADVANCED_FACE ( 'NONE', ( #16284 ), #770, .T. ) ;
#3985 = CARTESIAN_POINT ( 'NONE',  ( 34.91600907648203389, -11.88801210197604341, 11.56671555609732671 ) ) ;
#3986 = CIRCLE ( 'NONE', #10905, 10.50000000000000000 ) ;
#3987 = VERTEX_POINT ( 'NONE', #3670 ) ;
#3988 = CARTESIAN_POINT ( 'NONE',  ( 32.79901970863393501, -6.593096864778464017, 5.783357778048658915 ) ) ;
#3989 = CARTESIAN_POINT ( 'NONE',  ( 30.23341599105502908, -5.648260380436596506, -7.939653947423662927 ) ) ;
#3990 = CARTESIAN_POINT ( 'NONE',  ( 25.83973938098743517, -3.435034105423886874, -4.207126410816434792 ) ) ;
#3991 = CARTESIAN_POINT ( 'NONE',  ( 26.31556265977298992, -7.384422263489805793, -5.783357778048663356 ) ) ;
#3992 = CARTESIAN_POINT ( 'NONE',  ( 28.35948656569675919, -3.366149737736551906, -3.627061608673662896 ) ) ;
#3993 = CARTESIAN_POINT ( 'NONE',  ( 28.72045243349238675, -6.030415129707233035, -8.283357778048664244 ) ) ;
#3994 = CARTESIAN_POINT ( 'NONE',  ( 28.13873763417255347, -3.192873105281056390, -3.283357778048662023 ) ) ;
#3995 = CARTESIAN_POINT ( 'NONE',  ( 45.00000000000000711, -16.03270077640482683, -0.5379818257722508434 ) ) ;
#3996 = ADVANCED_FACE ( 'NONE', ( #9195 ), #6391, .F. ) ;
#3997 = CARTESIAN_POINT ( 'NONE',  ( 29.70732014299206369, -2.276983097582480742, -7.033357778048658027 ) ) ;
#3998 =( BOUNDED_CURVE ( )  B_SPLINE_CURVE ( 2, ( #4465, #1856, #4730, #2127, #15618, #3469, #17277, #9000, #3196 ),
 .UNSPECIFIED., .F., .T. ) 
 B_SPLINE_CURVE_WITH_KNOTS ( ( 3, 2, 2, 2, 3 ),
 ( 0.7115384615384615641, 0.7179487179487179516, 0.7307692307692307265, 0.7435897435897436125, 0.7500000000000000000 ),
 .UNSPECIFIED. ) 
 CURVE ( )  GEOMETRIC_REPRESENTATION_ITEM ( )  RATIONAL_B_SPLINE_CURVE ( ( 0.9330127018922194093, 0.9330127018922194093, 1.000000000000000000, 0.8660254037844387076, 1.000000000000000000, 0.8660254037844387076, 1.000000000000000000, 0.9330127018922194093, 0.9330127018922194093 ) ) 
 REPRESENTATION_ITEM ( '' )  );
#3999 = VECTOR ( 'NONE', #7881, 1000.000000000000114 ) ;
#4000 = EDGE_LOOP ( 'NONE', ( #14832, #4231, #11714, #6743 ) ) ;
#4001 = CARTESIAN_POINT ( 'NONE',  ( 32.14213199643172914, -2.910415664685331638, -3.627061608673662896 ) ) ;
#4002 = VECTOR ( 'NONE', #7489, 1000.000000000000000 ) ;
#4003 = FACE_OUTER_BOUND ( 'NONE', #13112, .T. ) ;
#4004 = CARTESIAN_POINT ( 'NONE',  ( 32.57506351453486815, -6.630276025878011126, -5.113484796970860558 ) ) ;
#4005 = DIRECTION ( 'NONE',  ( 0.000000000000000000, 0.000000000000000000, 1.000000000000000000 ) ) ;
#4006 = DIRECTION ( 'NONE',  ( -0.05980762113533058533, 0.4964101615137755386, 0.8660254037844385966 ) ) ;
#4007 = CARTESIAN_POINT ( 'NONE',  ( 29.60297508593253468, -5.724216059278466773, -7.939653947423662927 ) ) ;
#4008 = ORIENTED_EDGE ( 'NONE', *, *, #12945, .F. ) ;
#4009 = DIRECTION ( 'NONE',  ( -1.000000000000000000, 0.000000000000000000, 0.000000000000000000 ) ) ;
#4010 = CIRCLE ( 'NONE', #10365, 0.9000000000000011324 ) ;
#4011 = ORIENTED_EDGE ( 'NONE', *, *, #7966, .F. ) ;
#4012 = DIRECTION ( 'NONE',  ( -0.000000000000000000, -0.000000000000000000, 1.000000000000000000 ) ) ;
#4013 = ORIENTED_EDGE ( 'NONE', *, *, #9997, .F. ) ;
#4014 = CARTESIAN_POINT ( 'NONE',  ( 29.52399153675929355, -1.971908820246954130, -5.783357778048658915 ) ) ;
#4015 = EDGE_CURVE ( 'NONE', #17192, #17584, #4928, .T. ) ;
#4016 = PLANE ( 'NONE',  #4979 ) ;
#4017 = ORIENTED_EDGE ( 'NONE', *, *, #15259, .F. ) ;
#4018 =( BOUNDED_CURVE ( )  B_SPLINE_CURVE ( 2, ( #11431, #12987, #9093, #16995, #11619, #10255, #3197, #8736, #13079 ),
 .UNSPECIFIED., .F., .F. ) 
 B_SPLINE_CURVE_WITH_KNOTS ( ( 3, 2, 2, 2, 3 ),
 ( 0.09615384615384617306, 0.1025641025641025605, 0.1153846153846153910, 0.1282051282051281937, 0.1346153846153846367 ),
 .UNSPECIFIED. ) 
 CURVE ( )  GEOMETRIC_REPRESENTATION_ITEM ( )  RATIONAL_B_SPLINE_CURVE ( ( 0.9330127018922194093, 0.9330127018922196314, 1.000000000000000000, 0.8660254037844387076, 1.000000000000000000, 0.8660254037844387076, 1.000000000000000000, 0.9330127018922190762, 0.9330127018922194093 ) ) 
 REPRESENTATION_ITEM ( '' )  );
#4019 = CARTESIAN_POINT ( 'NONE',  ( 25.59340017005574097, -5.757764245108966783, -8.283357778048664244 ) ) ;
#4020 = CARTESIAN_POINT ( 'NONE',  ( -10.50000000000000000, 0.000000000000000000, -10.00000000000000000 ) ) ;
#4021 = CARTESIAN_POINT ( 'NONE',  ( 31.68992120585416217, -1.700760206360153015, 5.783357778048662468 ) ) ;
#4022 = CARTESIAN_POINT ( 'NONE',  ( 33.83155592109562804, -6.868441680671474536, -5.783357778048669573 ) ) ;
#4023 = VECTOR ( 'NONE', #14123, 1000.000000000000000 ) ;
#4024 = CARTESIAN_POINT ( 'NONE',  ( 0.000000000000000000, 0.000000000000000000, -8.722503561260788629 ) ) ;
#4025 = VECTOR ( 'NONE', #2595, 1000.000000000000000 ) ;
#4026 = CARTESIAN_POINT ( 'NONE',  ( 29.80442540930208750, -6.953886339277345563, 5.783357778048657138 ) ) ;
#4027 = FILL_AREA_STYLE ('',( #16293 ) ) ;
#4028 = CARTESIAN_POINT ( 'NONE',  ( 36.48725301720441649, 2.437776833296281698, -5.783357778048662468 ) ) ;
#4029 = ORIENTED_EDGE ( 'NONE', *, *, #11209, .T. ) ;
#4030 = ORIENTED_EDGE ( 'NONE', *, *, #16936, .F. ) ;
#4031 = VECTOR ( 'NONE', #11011, 1000.000000000000227 ) ;
#4032 = FACE_OUTER_BOUND ( 'NONE', #11264, .T. ) ;
#4033 = ADVANCED_FACE ( 'NONE', ( #6649 ), #9188, .T. ) ;
#4034 = DIRECTION ( 'NONE',  ( -0.7071067811865462405, 0.000000000000000000, -0.7071067811865489050 ) ) ;
#4035 = CARTESIAN_POINT ( 'NONE',  ( 30.17635249042624679, -2.520282741259753045, -6.861505862736158257 ) ) ;
#4036 = DIRECTION ( 'NONE',  ( 0.9928203230275510771, 0.1196152422706609902, 4.006172263299092517E-17 ) ) ;
#4037 = CARTESIAN_POINT ( 'NONE',  ( 30.00264913441657555, -6.940201157507134511, 5.783357778048669573 ) ) ;
#4038 = DIRECTION ( 'NONE',  ( -0.9237280213470682178, -0.3830490080632377725, 0.000000000000000000 ) ) ;
#4039 = CARTESIAN_POINT ( 'NONE',  ( 26.25801688195511474, -3.619335333876111171, 3.627061608673666893 ) ) ;
#4040 = VECTOR ( 'NONE', #15896, 1000.000000000000114 ) ;
#4041 = PRODUCT_DEFINITION_SHAPE ( 'NONE', 'NONE',  #17978 ) ;
#4042 = CARTESIAN_POINT ( 'NONE',  ( 27.51889869220010354, -3.467423976192371082, 3.627061608673666893 ) ) ;
#4043 = DIRECTION ( 'NONE',  ( 0.9928203230275512992, 0.1196152422706610180, 4.006172263299093133E-17 ) ) ;
#4044 = LINE ( 'NONE', #6511, #11214 ) ;
#4045 = ADVANCED_FACE ( 'NONE', ( #7845 ), #4829, .F. ) ;
#4046 = CARTESIAN_POINT ( 'NONE',  ( 32.80318959510331212, -2.203800746085299522, 6.861505862736166250 ) ) ;
#4047 = AXIS2_PLACEMENT_3D ( 'NONE', #5466, #15185, #6927 ) ;
#4048 = ORIENTED_EDGE ( 'NONE', *, *, #15785, .T. ) ;
#4049 = ORIENTED_EDGE ( 'NONE', *, *, #5721, .F. ) ;
#4050 = ORIENTED_EDGE ( 'NONE', *, *, #11786, .T. ) ;
#4051 = CARTESIAN_POINT ( 'NONE',  ( 30.64918316926811315, -2.463315982128351678, 4.705209693361167567 ) ) ;
#4052 = CARTESIAN_POINT ( 'NONE',  ( 29.45101334415624095, -7.006662376286320715, -5.783357778048657138 ) ) ;
#4053 = VERTEX_POINT ( 'NONE', #15175 ) ;
#4054 = AXIS2_PLACEMENT_3D ( 'NONE', #8842, #15368, #5926 ) ;
#4055 = CARTESIAN_POINT ( 'NONE',  ( 28.39010325924584421, -2.735490497978389612, 6.861505862736166250 ) ) ;
#4056 = DIRECTION ( 'NONE',  ( 1.000000000000000000, 0.000000000000000000, 0.000000000000000000 ) ) ;
#4057 = CARTESIAN_POINT ( 'NONE',  ( 0.000000000000000000, 0.000000000000000000, -4.000000000000000000 ) ) ;
#4058 = CARTESIAN_POINT ( 'NONE',  ( 28.56587103547553852, -2.077146556768465047, 6.453230759126474148 ) ) ;
#4059 = CARTESIAN_POINT ( 'NONE',  ( 27.25621498173240198, -3.499072175709823984, -3.627061608673662008 ) ) ;
#4060 = DIRECTION ( 'NONE',  ( 0.6000000000000001998, 0.7999999999999999334, 0.000000000000000000 ) ) ;
#4061 = VERTEX_POINT ( 'NONE', #2833 ) ;
#4063 = ADVANCED_FACE ( 'NONE', ( #9537 ), #16612, .F. ) ;
#4062 = CARTESIAN_POINT ( 'NONE',  ( 31.20090818012769773, -4.277755612481361602, -8.283357778048662468 ) ) ;
#4064 = DIRECTION ( 'NONE',  ( -0.1196152422706611984, 0.9928203230275510771, 0.000000000000000000 ) ) ;
#4065 = PLANE ( 'NONE',  #13294 ) ;
#4066 = DIRECTION ( 'NONE',  ( -0.1196152422706584506, 0.9928203230275515212, 0.000000000000000000 ) ) ;
#4067 = CARTESIAN_POINT ( 'NONE',  ( 29.80442540930208750, -6.953886339277345563, -5.783357778048669573 ) ) ;
#4068 = CIRCLE ( 'NONE', #6967, 2.499999999999999556 ) ;
#4069 = EDGE_CURVE ( 'NONE', #15072, #2226, #11486, .T. ) ;
#4070 = CARTESIAN_POINT ( 'NONE',  ( 27.65458886993626564, -2.824105456627233224, -6.861505862736158257 ) ) ;
#4071 = ORIENTED_EDGE ( 'NONE', *, *, #16962, .T. ) ;
#4072 = DIRECTION ( 'NONE',  ( -0.9928203230275514102, -0.1196152422706598939, 0.000000000000000000 ) ) ;
#4073 = DIRECTION ( 'NONE',  ( -0.000000000000000000, -0.000000000000000000, -1.000000000000000000 ) ) ;
#4074 = EDGE_LOOP ( 'NONE', ( #7114, #11534, #12477, #8643 ) ) ;
#4075 = CARTESIAN_POINT ( 'NONE',  ( 31.39792096211754924, -4.254019462947003838, 3.627061608673664228 ) ) ;
#4076 = CARTESIAN_POINT ( 'NONE',  ( 28.25893984004492765, -6.513116296623863377, -4.705209693361168455 ) ) ;
#4077 = LINE ( 'NONE', #15144, #3170 ) ;
#4078 = LINE ( 'NONE', #2546, #3229 ) ;
#4079 = CARTESIAN_POINT ( 'NONE',  ( 27.60205212784272177, -2.830435096530727446, -4.705209693361161349 ) ) ;
#4080 = FACE_OUTER_BOUND ( 'NONE', #4673, .T. ) ;
#4081 = FACE_OUTER_BOUND ( 'NONE', #782, .T. ) ;
#4082 = CIRCLE ( 'NONE', #10723, 2.500000000000000888 ) ;
#4083 = ADVANCED_FACE ( 'NONE', ( #8197 ), #15347, .T. ) ;
#4084 = DIRECTION ( 'NONE',  ( 0.9928203230275510771, 0.1196152422706609902, 4.006172263299092517E-17 ) ) ;
#4085 = UNCERTAINTY_MEASURE_WITH_UNIT (LENGTH_MEASURE( 1.000000000000000082E-05 ), #10847, 'distance_accuracy_value', 'NONE');
#4086 = CARTESIAN_POINT ( 'NONE',  ( 29.77118727536320719, -5.903822331637461396, -3.283357778048667797 ) ) ;
#4087 = VECTOR ( 'NONE', #12683, 1000.000000000000000 ) ;
#4088 = ORIENTED_EDGE ( 'NONE', *, *, #11765, .F. ) ;
#4089 = EDGE_LOOP ( 'NONE', ( #7110, #11157, #11633, #17145, #10471, #8655 ) ) ;
#4090 = FACE_OUTER_BOUND ( 'NONE', #5029, .T. ) ;
#4091 = EDGE_CURVE ( 'NONE', #13220, #14372, #2574, .T. ) ;
#4092 = CARTESIAN_POINT ( 'NONE',  ( 27.92859066579839222, -3.218191664895003523, -8.283357778048660691 ) ) ;
#4093 = CARTESIAN_POINT ( 'NONE',  ( 25.71748644841968456, -2.420320648352046078, -5.783357778048663356 ) ) ;
#4094 = DIRECTION ( 'NONE',  ( 1.000000000000000000, 0.000000000000000000, 0.000000000000000000 ) ) ;
#4095 = CARTESIAN_POINT ( 'NONE',  ( -1.274241539467094064, -3.883118457693087500, -2.920601398289341954 ) ) ;
#4096 = CARTESIAN_POINT ( 'NONE',  ( 29.49337484321020497, -2.602568060005117090, -4.705209693361161349 ) ) ;
#4097 = CIRCLE ( 'NONE', #17745, 0.9000000000000003553 ) ;
#4098 = AXIS2_PLACEMENT_3D ( 'NONE', #14805, #5000, #13444 ) ;
#4099 = EDGE_CURVE ( 'NONE', #1198, #579, #8316, .T. ) ;
#4100 = FACE_OUTER_BOUND ( 'NONE', #14740, .T. ) ;
#4101 = CARTESIAN_POINT ( 'NONE',  ( 0.000000000000000000, 0.000000000000000000, -12.00000000000000000 ) ) ;
#4102 = AXIS2_PLACEMENT_3D ( 'NONE', #13720, #10704, #5276 ) ;
#4103 = CIRCLE ( 'NONE', #9881, 10.50000000000000000 ) ;
#4104 = CARTESIAN_POINT ( 'NONE',  ( 6.935828204433864386, -17.68137362934027124, -16.94363565911716663 ) ) ;
#4105 = VERTEX_POINT ( 'NONE', #9623 ) ;
#4106 =( BOUNDED_CURVE ( )  B_SPLINE_CURVE ( 2, ( #14864, #2452, #13679, #1080, #6602, #17713, #2712, #5232, #1267 ),
 .UNSPECIFIED., .F., .T. ) 
 B_SPLINE_CURVE_WITH_KNOTS ( ( 3, 2, 2, 2, 3 ),
 ( 0.1730769230769231004, 0.1794871794871794879, 0.1923076923076923184, 0.2051282051282051211, 0.2115384615384615641 ),
 .UNSPECIFIED. ) 
 CURVE ( )  GEOMETRIC_REPRESENTATION_ITEM ( )  RATIONAL_B_SPLINE_CURVE ( ( 0.9330127018922194093, 0.9330127018922196314, 1.000000000000000000, 0.8660254037844387076, 1.000000000000000000, 0.8660254037844387076, 1.000000000000000000, 0.9330127018922190762, 0.9330127018922194093 ) ) 
 REPRESENTATION_ITEM ( '' )  );
#4107 = EDGE_CURVE ( 'NONE', #1572, #17008, #13634, .T. ) ;
#4108 = CARTESIAN_POINT ( 'NONE',  ( 31.06530721954707985, -6.801974981593605918, -5.783357778048669573 ) ) ;
#4109 = DIRECTION ( 'NONE',  ( 1.000000000000000000, 0.000000000000000000, 0.000000000000000000 ) ) ;
#4110 = AXIS2_PLACEMENT_3D ( 'NONE', #3921, #5440, #3838 ) ;
#4111 = ORIENTED_EDGE ( 'NONE', *, *, #17646, .F. ) ;
#4112 = CARTESIAN_POINT ( 'NONE',  ( 32.34358231980129261, -4.140085944684206432, -3.627061608673664672 ) ) ;
#4113 = FACE_OUTER_BOUND ( 'NONE', #6615, .T. ) ;
#4114 = CARTESIAN_POINT ( 'NONE',  ( 4.000000000000000000, 2.472263363263126124, -3.387027814857423991 ) ) ;
#4115 = CARTESIAN_POINT ( 'NONE',  ( 26.65222088368961195, -7.333664733486695120, -5.783357778048669573 ) ) ;
#4116 = CIRCLE ( 'NONE', #5846, 0.8000000000000003775 ) ;
#4117 = EDGE_LOOP ( 'NONE', ( #10813, #14996 ) ) ;
#4118 = CARTESIAN_POINT ( 'NONE',  ( 25.01460733971720529, -22.13799366862516038, -14.47321228143779415 ) ) ;
#4119 = EDGE_CURVE ( 'NONE', #4053, #11016, #4210, .T. ) ;
#4120 = VECTOR ( 'NONE', #9651, 1000.000000000000000 ) ;
#4121 = CARTESIAN_POINT ( 'NONE',  ( 26.19678349485696955, -4.880653813392439311, 7.939653947423662039 ) ) ;
#4122 = DIRECTION ( 'NONE',  ( -1.000000000000000000, 0.000000000000000000, 0.000000000000000000 ) ) ;
#4123 = CARTESIAN_POINT ( 'NONE',  ( 28.43075721014566781, -2.093425104433228157, 5.113484796970856117 ) ) ;
#4124 = ORIENTED_EDGE ( 'NONE', *, *, #5854, .T. ) ;
#4125 = AXIS2_PLACEMENT_3D ( 'NONE', #15186, #16548, #8289 ) ;
#4126 = CARTESIAN_POINT ( 'NONE',  ( 28.74176732417158320, -7.092112515190875044, -5.783357778048657138 ) ) ;
#4127 = ORIENTED_EDGE ( 'NONE', *, *, #14940, .F. ) ;
#4128 = CARTESIAN_POINT ( 'NONE',  ( 27.22618411036838637, -2.238552374514887866, -5.113484796970851676 ) ) ;
#4129 =( BOUNDED_CURVE ( )  B_SPLINE_CURVE ( 2, ( #16649, #3047, #2775, #141, #5836, #13915, #9915, #8296, #12733 ),
 .UNSPECIFIED., .F., .T. ) 
 B_SPLINE_CURVE_WITH_KNOTS ( ( 3, 2, 2, 2, 3 ),
 ( 0.3653846153846154188, 0.3717948717948718063, 0.3846153846153846367, 0.3974358974358974117, 0.4038461538461538547 ),
 .UNSPECIFIED. ) 
 CURVE ( )  GEOMETRIC_REPRESENTATION_ITEM ( )  RATIONAL_B_SPLINE_CURVE ( ( 0.9330127018922194093, 0.9330127018922196314, 1.000000000000000000, 0.8660254037844387076, 1.000000000000000000, 0.8660254037844387076, 1.000000000000000000, 0.9330127018922190762, 0.9330127018922194093 ) ) 
 REPRESENTATION_ITEM ( '' )  );
#4130 = ORIENTED_EDGE ( 'NONE', *, *, #14174, .T. ) ;
#4131 = CARTESIAN_POINT ( 'NONE',  ( 0.000000000000000000, 0.000000000000000000, -1.901951201008075243 ) ) ;
#4132 = ADVANCED_FACE ( 'NONE', ( #12539 ), #1224, .F. ) ;
#4133 = CARTESIAN_POINT ( 'NONE',  ( 28.40332666278570173, -4.614808937445885384, -7.939653947423662039 ) ) ;
#4134 = UNCERTAINTY_MEASURE_WITH_UNIT (LENGTH_MEASURE( 1.000000000000000082E-05 ), #12860, 'distance_accuracy_value', 'NONE');
#4135 = DIRECTION ( 'NONE',  ( 0.000000000000000000, 0.000000000000000000, -1.000000000000000000 ) ) ;
#4136 = VECTOR ( 'NONE', #6127, 1000.000000000000227 ) ;
#4137 = DIRECTION ( 'NONE',  ( 0.000000000000000000, 0.000000000000000000, -1.000000000000000000 ) ) ;
#4138 = DIRECTION ( 'NONE',  ( -1.000000000000000000, 0.000000000000000000, 0.000000000000000000 ) ) ;
#4139 = CARTESIAN_POINT ( 'NONE',  ( 29.81991338116587542, -2.990324628369393611, -8.283357778048660691 ) ) ;
#4140 = CARTESIAN_POINT ( 'NONE',  ( 30.76748005699505129, -4.329975141788874993, 3.627061608673664228 ) ) ;
#4141 = AXIS2_PLACEMENT_3D ( 'NONE', #2141, #2042, #11634 ) ;
#4142 = CARTESIAN_POINT ( 'NONE',  ( -14.00000000000000178, 0.000000000000000000, 8.700000000000001066 ) ) ;
#4143 = CARTESIAN_POINT ( 'NONE',  ( 26.10855331130634127, -2.710563430764044490, -4.533357778048659803 ) ) ;
#4144 = CARTESIAN_POINT ( 'NONE',  ( 33.54323074294813267, -5.249493066516778050, 3.627061608673662896 ) ) ;
#4145 = AXIS2_PLACEMENT_3D ( 'NONE', #11905, #7929, #17488 ) ;
#4146 = VECTOR ( 'NONE', #12919, 1000.000000000000114 ) ;
#4147 = EDGE_CURVE ( 'NONE', #11147, #14109, #3986, .T. ) ;
#4148 = EDGE_LOOP ( 'NONE', ( #10683, #4253, #12480, #15877 ) ) ;
#4149 = ADVANCED_FACE ( 'NONE', ( #33 ), #5542, .F. ) ;
#4150 = ORIENTED_EDGE ( 'NONE', *, *, #17037, .F. ) ;
#4151 = CARTESIAN_POINT ( 'NONE',  ( 26.97161122272022382, -2.906390775372597712, 6.861505862736165362 ) ) ;
#4152 = AXIS2_PLACEMENT_3D ( 'NONE', #10385, #10640, #13026 ) ;
#4153 = FACE_OUTER_BOUND ( 'NONE', #921, .T. ) ;
#4154 = ORIENTED_EDGE ( 'NONE', *, *, #1019, .T. ) ;
#4155 = CARTESIAN_POINT ( 'NONE',  ( 27.00222791626931240, -2.275731535614434531, 5.783357778048668685 ) ) ;
#4156 = ORIENTED_EDGE ( 'NONE', *, *, #15646, .F. ) ;
#4157 = CARTESIAN_POINT ( 'NONE',  ( 30.95252083063564896, -1.789602389065743981, -6.453230759126464378 ) ) ;
#4158 = LINE ( 'NONE', #13586, #15914 ) ;
#4159 = CIRCLE ( 'NONE', #6747, 2.500000000000001776 ) ;
#4160 = CARTESIAN_POINT ( 'NONE',  ( 26.03726795043090547, -3.446058701420613879, -8.283357778048660691 ) ) ;
#4161 = AXIS2_PLACEMENT_3D ( 'NONE', #16875, #8328, #269 ) ;
#4162 = PLANE ( 'NONE',  #8729 ) ;
#4163 = CARTESIAN_POINT ( 'NONE',  ( 29.15568435273173264, -2.343444316361667834, -7.033357778048658027 ) ) ;
#4164 = DIRECTION ( 'NONE',  ( -1.000000000000000000, 1.224646799147352714E-16, 0.000000000000000000 ) ) ;
#4165 = CARTESIAN_POINT ( 'NONE',  ( 17.59269349951685157, -13.05689734314391970, -15.91118832497637570 ) ) ;
#4166 = CARTESIAN_POINT ( 'NONE',  ( 27.11150007966593733, -11.49307575575171469, 13.95470972894434780 ) ) ;
#4167 = VERTEX_POINT ( 'NONE', #15721 ) ;
#4168 = CARTESIAN_POINT ( 'NONE',  ( 29.54591158530375239, -2.596238420101622868, -6.861505862736158257 ) ) ;
#4169 = CARTESIAN_POINT ( 'NONE',  ( 28.89355063163679915, -2.047864499088824175, -5.783357778048658915 ) ) ;
#4170 = CARTESIAN_POINT ( 'NONE',  ( 33.18226487515251222, -2.585227674546096033, 8.283357778048664244 ) ) ;
#4171 = CARTESIAN_POINT ( 'NONE',  ( 41.90164972253718645, -2.988527579590353422, -5.783357778048662468 ) ) ;
#4172 = EDGE_LOOP ( 'NONE', ( #2696, #9296, #8373, #746 ) ) ;
#4173 = EDGE_CURVE ( 'NONE', #2932, #29, #1091, .T. ) ;
#4174 = ORIENTED_EDGE ( 'NONE', *, *, #8934, .T. ) ;
#4175 = CARTESIAN_POINT ( 'NONE',  ( 32.01513846370018967, -2.298745344637636912, 6.861505862736165362 ) ) ;
#4176 = CARTESIAN_POINT ( 'NONE',  ( 30.02326902268086428, -5.673578940050561847, -3.627061608673667781 ) ) ;
#4177 = CARTESIAN_POINT ( 'NONE',  ( 29.16815758536418102, -2.004582921727632971, -5.783357778048664244 ) ) ;
#4178 = CARTESIAN_POINT ( 'NONE',  ( 25.92409770820621162, -4.135217962343409326, -3.765474553462066165 ) ) ;
#4179 = CARTESIAN_POINT ( 'NONE',  ( 28.76917853929504432, -3.116917426439186123, -3.283357778048662023 ) ) ;
#4180 = CARTESIAN_POINT ( 'NONE',  ( 27.61527553138257574, -4.709753535998224550, -7.939653947423662039 ) ) ;
#4181 = CARTESIAN_POINT ( 'NONE',  ( 26.24741491880506672, -3.420740141806666301, -3.283357778048662023 ) ) ;
#4182 = ADVANCED_FACE ( 'NONE', ( #5814, #13080, #11620 ), #7555, .T. ) ;
#4183 = FACE_OUTER_BOUND ( 'NONE', #16924, .T. ) ;
#4184 = CARTESIAN_POINT ( 'NONE',  ( 28.48022645605872327, -3.151730446115816875, -8.283357778048658915 ) ) ;
#4185 = CARTESIAN_POINT ( 'NONE',  ( 31.53813789838894621, -6.745008222462202774, -5.783357778048668685 ) ) ;
#4186 = DIRECTION ( 'NONE',  ( -0.9928203230275514102, -0.1196152422706598939, -0.000000000000000000 ) ) ;
#4187 = PLANE ( 'NONE',  #15857 ) ;
#4188 = LINE ( 'NONE', #13876, #15131 ) ;
#4189 = CARTESIAN_POINT ( 'NONE',  ( -2.742797192660360484, -3.035247456001994859, -3.133250573521795257 ) ) ;
#4190 = CARTESIAN_POINT ( 'NONE',  ( 27.62849893492243325, -6.589071975465733644, -4.705209693361168455 ) ) ;
#4191 = EDGE_CURVE ( 'NONE', #14530, #1198, #7387, .T. ) ;
#4192 = EDGE_LOOP ( 'NONE', ( #14114, #14791, #14320, #11733 ) ) ;
#4193 = VERTEX_POINT ( 'NONE', #12710 ) ;
#4194 = CARTESIAN_POINT ( 'NONE',  ( 45.00000000000000711, -19.03270077640482683, 10.53798182577225084 ) ) ;
#4195 = CARTESIAN_POINT ( 'NONE',  ( 0.000000000000000000, 0.000000000000000000, -9.600000000000001421 ) ) ;
#4196 = ORIENTED_EDGE ( 'NONE', *, *, #2189, .F. ) ;
#4197 = CARTESIAN_POINT ( 'NONE',  ( -45.50000000000000000, -19.03270077640483038, 5.537981825772250843 ) ) ;
#4198 = ORIENTED_EDGE ( 'NONE', *, *, #8588, .T. ) ;
#4199 = EDGE_CURVE ( 'NONE', #4757, #4277, #8638, .T. ) ;
#4200 = CARTESIAN_POINT ( 'NONE',  ( 30.15443244188179150, -1.895953141405083864, -5.783357778048658915 ) ) ;
#4201 = DIRECTION ( 'NONE',  ( -0.000000000000000000, -0.000000000000000000, 1.000000000000000000 ) ) ;
#4202 = ORIENTED_EDGE ( 'NONE', *, *, #7943, .T. ) ;
#4203 = CARTESIAN_POINT ( 'NONE',  ( 31.49429780130001433, -5.496349022752856861, -7.939653947423664704 ) ) ;
#4204 = CARTESIAN_POINT ( 'NONE',  ( 0.000000000000000000, 0.000000000000000000, 0.000000000000000000 ) ) ;
#4205 = DIRECTION ( 'NONE',  ( 0.9928203230275512992, 0.1196152422706610180, 4.006172263299093133E-17 ) ) ;
#4206 = CARTESIAN_POINT ( 'NONE',  ( 27.63266882139180680, -2.199775856772564708, -5.783357778048658027 ) ) ;
#4207 = CARTESIAN_POINT ( 'NONE',  ( 41.90164972253716513, -2.988527579590351646, -5.783357778048662468 ) ) ;
#4208 = ORIENTED_EDGE ( 'NONE', *, *, #4934, .T. ) ;
#4209 = EDGE_CURVE ( 'NONE', #14073, #17902, #6052, .T. ) ;
#4210 =( BOUNDED_CURVE ( )  B_SPLINE_CURVE ( 2, ( #15255, #210, #6914, #10974, #16628, #5719, #13996, #5455, #4021 ),
 .UNSPECIFIED., .F., .T. ) 
 B_SPLINE_CURVE_WITH_KNOTS ( ( 3, 2, 2, 2, 3 ),
 ( 0.1346153846153846367, 0.1410256410256410242, 0.1538461538461538547, 0.1666666666666666574, 0.1730769230769231004 ),
 .UNSPECIFIED. ) 
 CURVE ( )  GEOMETRIC_REPRESENTATION_ITEM ( )  RATIONAL_B_SPLINE_CURVE ( ( 0.9330127018922194093, 0.9330127018922196314, 1.000000000000000000, 0.8660254037844387076, 1.000000000000000000, 0.8660254037844387076, 1.000000000000000000, 0.9330127018922190762, 0.9330127018922194093 ) ) 
 REPRESENTATION_ITEM ( '' )  );
#4211 = CARTESIAN_POINT ( 'NONE',  ( 37.87429945334753256, 1.178459718517443022, -5.783357778048661579 ) ) ;
#4212 = CARTESIAN_POINT ( 'NONE',  ( 9.099998387031005720, -19.29508120620799971, 16.81964500401478091 ) ) ;
#4213 = CARTESIAN_POINT ( 'NONE',  ( 32.97211790677835097, -2.610546234160043610, 3.283357778048666464 ) ) ;
#4214 = ORIENTED_EDGE ( 'NONE', *, *, #10326, .F. ) ;
#4215 = CARTESIAN_POINT ( 'NONE',  ( 28.79925754835455010, -6.020920669644549861, 3.283357778048663356 ) ) ;
#4216 = DIRECTION ( 'NONE',  ( 0.5595328448060640225, 0.8288081777970298658, -3.349091179051939016E-15 ) ) ;
#4217 = ORIENTED_EDGE ( 'NONE', *, *, #5069, .F. ) ;
#4218 = DIRECTION ( 'NONE',  ( -0.9928203230275514102, -0.1196152422706598939, 0.000000000000000000 ) ) ;
#4219 = CARTESIAN_POINT ( 'NONE',  ( 25.99533317148741318, -3.650983533393564517, -3.627061608673662008 ) ) ;
#4220 = ADVANCED_FACE ( 'NONE', ( #7464 ), #4732, .T. ) ;
#4221 = DIRECTION ( 'NONE',  ( 0.1196152422706605323, -0.9928203230275512992, 0.000000000000000000 ) ) ;
#4222 = CARTESIAN_POINT ( 'NONE',  ( 0.000000000000000000, 0.000000000000000000, -3.700000000000000178 ) ) ;
#4223 = DIRECTION ( 'NONE',  ( 0.000000000000000000, 0.000000000000000000, 1.000000000000000000 ) ) ;
#4224 = CARTESIAN_POINT ( 'NONE',  ( 33.50243880635947846, -1.482387629897225390, 5.783357778048663356 ) ) ;
#4225 = CARTESIAN_POINT ( 'NONE',  ( 28.34209327568754233, -5.876127416962207306, 3.627061608673662896 ) ) ;
#4226 = DIRECTION ( 'NONE',  ( 0.9928203230275510771, 0.1196152422706614621, -0.000000000000000000 ) ) ;
#4227 = CARTESIAN_POINT ( 'NONE',  ( 25.76466184735054910, -2.811881907026620553, 5.318565573966401061 ) ) ;
#4228 = EDGE_CURVE ( 'NONE', #6312, #12121, #11432, .T. ) ;
#4229 = VERTEX_POINT ( 'NONE', #4467 ) ;
#4230 = B_SPLINE_CURVE_WITH_KNOTS ( 'NONE', 3,
 ( #1807, #11470, #3243, #12662, #12855 ),
 .UNSPECIFIED., .F., .F.,
 ( 4, 1, 4 ),
 ( 0.000000000000000000, 0.002309401076758504923, 0.004618802153517009845 ),
 .UNSPECIFIED. ) ;
#4231 = ORIENTED_EDGE ( 'NONE', *, *, #16185, .T. ) ;
#4232 = CARTESIAN_POINT ( 'NONE',  ( 28.88938074516742205, -6.437160617781993999, 6.861505862736158257 ) ) ;
#4233 = CARTESIAN_POINT ( 'NONE',  ( 27.32822876973539294, -6.198150586942257512, 8.283357778048660691 ) ) ;
#4234 = ORIENTED_EDGE ( 'NONE', *, *, #9787, .T. ) ;
#4235 = CARTESIAN_POINT ( 'NONE',  ( 25.76466184735054910, -2.811881907026620553, 5.318565573966400173 ) ) ;
#4236 = ORIENTED_EDGE ( 'NONE', *, *, #15879, .T. ) ;
#4237 = ORIENTED_EDGE ( 'NONE', *, *, #11089, .F. ) ;
#4238 = CARTESIAN_POINT ( 'NONE',  ( 2.540000000000001368, 0.000000000000000000, 1.599999999999998979 ) ) ;
#4239 = DIRECTION ( 'NONE',  ( 1.000000000000000000, 0.000000000000000000, 0.000000000000000000 ) ) ;
#4240 = DIRECTION ( 'NONE',  ( -0.000000000000000000, -0.000000000000000000, 1.000000000000000000 ) ) ;
#4241 = CARTESIAN_POINT ( 'NONE',  ( 26.41562710823574278, -3.600346414165641828, -7.939653947423660263 ) ) ;
#4242 = LINE ( 'NONE', #10271, #13073 ) ;
#4243 = APPLICATION_CONTEXT ( 'automotive_design' ) ;
#4244 = CARTESIAN_POINT ( 'NONE',  ( 29.42969845347704450, -5.944964990802679594, -8.283357778048662468 ) ) ;
#4245 = CARTESIAN_POINT ( 'NONE',  ( 31.84257795004536007, -2.746633492292519296, -3.283357778048662023 ) ) ;
#4246 = ADVANCED_FACE ( 'NONE', ( #8913 ), #8827, .F. ) ;
#4247 = CARTESIAN_POINT ( 'NONE',  ( 27.69360539047986336, -12.07076363665953345, -13.80168160306295810 ) ) ;
#4248 = LINE ( 'NONE', #9748, #11358 ) ;
#4249 = CARTESIAN_POINT ( 'NONE',  ( 31.51169109130924184, -2.986371343527201905, -3.627061608673662896 ) ) ;
#4250 = ORIENTED_EDGE ( 'NONE', *, *, #17816, .T. ) ;
#4251 = CARTESIAN_POINT ( 'NONE',  ( 27.86926259684567597, -5.933094176093607786, -7.939653947423662927 ) ) ;
#4252 = FACE_OUTER_BOUND ( 'NONE', #12699, .T. ) ;
#4253 = ORIENTED_EDGE ( 'NONE', *, *, #9016, .T. ) ;
#4254 = EDGE_LOOP ( 'NONE', ( #6588, #9011, #7077, #4935 ) ) ;
#4255 = ORIENTED_EDGE ( 'NONE', *, *, #9354, .F. ) ;
#4256 = CARTESIAN_POINT ( 'NONE',  ( 29.51982165028991645, -6.361204938940122844, 6.861505862736158257 ) ) ;
#4257 = VERTEX_POINT ( 'NONE', #8549 ) ;
#4258 = CARTESIAN_POINT ( 'NONE',  ( 31.07327543742414022, -2.112412460091767308, 7.033357778048666020 ) ) ;
#4259 = DIRECTION ( 'NONE',  ( -0.1196152422706597551, 0.9928203230275514102, 0.000000000000000000 ) ) ;
#4260 = AXIS2_PLACEMENT_3D ( 'NONE', #14151, #8721, #12887 ) ;
#4261 = PLANE ( 'NONE',  #853 ) ;
#4262 = CARTESIAN_POINT ( 'NONE',  ( 25.07353123778398896, 1.235291682954687165, -14.60266621045498425 ) ) ;
#4263 = CARTESIAN_POINT ( 'NONE',  ( 28.10549950023366961, -2.142809097641162897, -5.783357778048658027 ) ) ;
#4264 = CARTESIAN_POINT ( 'NONE',  ( 5.000000000000000888, 0.000000000000000000, 0.000000000000000000 ) ) ;
#4265 = DIRECTION ( 'NONE',  ( 0.9928203230275512992, 0.1196152422706610180, 4.006172263299093133E-17 ) ) ;
#4266 = FACE_OUTER_BOUND ( 'NONE', #14255, .T. ) ;
#4267 = EDGE_CURVE ( 'NONE', #14747, #7654, #8909, .T. ) ;
#4268 = CARTESIAN_POINT ( 'NONE',  ( 27.81599742762458050, -2.504850134108091098, -7.033357778048658027 ) ) ;
#4269 = EDGE_LOOP ( 'NONE', ( #14110, #4481 ) ) ;
#4270 = CARTESIAN_POINT ( 'NONE',  ( 32.04158527077989760, -6.057382223572642665, -4.705209693361168455 ) ) ;
#4271 = CYLINDRICAL_SURFACE ( 'NONE', #8152, 13.00000000000000178 ) ;
#4272 = CARTESIAN_POINT ( 'NONE',  ( 26.58890374069123652, -3.379597482641427231, -8.283357778048660691 ) ) ;
#4273 = CARTESIAN_POINT ( 'NONE',  ( -0.1410420225375869918, 4.700232803196136011, -3.387027626239166089 ) ) ;
#4274 = CARTESIAN_POINT ( 'NONE',  ( 31.43732351782677625, -4.249272233123119413, 8.283357778048662468 ) ) ;
#4275 = CARTESIAN_POINT ( 'NONE',  ( 27.73357241910951743, -6.576412695658750529, -6.861505862736166250 ) ) ;
#4276 = ORIENTED_EDGE ( 'NONE', *, *, #5477, .F. ) ;
#4277 = VERTEX_POINT ( 'NONE', #7200 ) ;
#4278 = DIRECTION ( 'NONE',  ( 0.9928203230275512992, 0.1196152422706610180, 4.006172263299093133E-17 ) ) ;
#4279 = CARTESIAN_POINT ( 'NONE',  ( 28.19013153391124860, -7.158573733970061248, -5.783357778048657138 ) ) ;
#4280 = CARTESIAN_POINT ( 'NONE',  ( -21.03265992632394799, -10.27181489424398997, -15.32141966295701430 ) ) ;
#4281 = VERTEX_POINT ( 'NONE', #14359 ) ;
#4282 = AXIS2_PLACEMENT_3D ( 'NONE', #15262, #16541, #9805 ) ;
#4283 = CARTESIAN_POINT ( 'NONE',  ( 31.44176105920648112, -5.502678662656354192, -3.627061608673668225 ) ) ;
#4284 = CARTESIAN_POINT ( 'NONE',  ( 4.081988505578530102, 17.67880197223097127, 16.99999999999999645 ) ) ;
#4285 = EDGE_CURVE ( 'NONE', #7229, #11807, #13826, .T. ) ;
#4286 = CARTESIAN_POINT ( 'NONE',  ( 32.12473870642251939, -5.420393343910986594, -7.939653947423664704 ) ) ;
#4287 = CARTESIAN_POINT ( 'NONE',  ( 29.84999239022537409, -5.894327871574777333, 8.283357778048660691 ) ) ;
#4288 = CARTESIAN_POINT ( 'NONE',  ( 4.000000000000000000, -0.8732118962410247986, -2.923153487222570401 ) ) ;
#4289 = CARTESIAN_POINT ( 'NONE',  ( 29.81239362717914787, -2.264323817775507397, -4.533357778048659803 ) ) ;
#4290 = CARTESIAN_POINT ( 'NONE',  ( 16.75000000000000000, -16.21813761408365195, -16.03574476417184513 ) ) ;
#4291 = ORIENTED_EDGE ( 'NONE', *, *, #785, .F. ) ;
#4292 = CARTESIAN_POINT ( 'NONE',  ( 27.99987602667382802, -2.482696394238434578, 7.033357778048666020 ) ) ;
#4293 = EDGE_CURVE ( 'NONE', #13470, #3035, #15571, .T. ) ;
#4294 = CIRCLE ( 'NONE', #13839, 2.749999999999988454 ) ;
#4295 = VECTOR ( 'NONE', #9727, 1000.000000000000000 ) ;
#4296 = CARTESIAN_POINT ( 'NONE',  ( 27.75966235412334981, -2.811446176820259879, 6.861505862736166250 ) ) ;
#4297 = CARTESIAN_POINT ( 'NONE',  ( 23.00000000000000000, -16.21813761408365195, -13.00000000000000178 ) ) ;
#4298 = ORIENTED_EDGE ( 'NONE', *, *, #13736, .T. ) ;
#4299 = CARTESIAN_POINT ( 'NONE',  ( 26.31284730449749532, -7.327874027665321144, -6.311983372246984914 ) ) ;
#4300 = ORIENTED_EDGE ( 'NONE', *, *, #12281, .F. ) ;
#4301 = CARTESIAN_POINT ( 'NONE',  ( 26.63392073224175505, -2.647267031729148012, 4.533357778048667797 ) ) ;
#4302 = ORIENTED_EDGE ( 'NONE', *, *, #13999, .F. ) ;
#4303 = FACE_OUTER_BOUND ( 'NONE', #14284, .T. ) ;
#4304 = CARTESIAN_POINT ( 'NONE',  ( 28.52162355051263987, -6.481468097106410475, -6.861505862736167138 ) ) ;
#4305 = AXIS2_PLACEMENT_3D ( 'NONE', #8952, #13126, #705 ) ;
#4306 = ADVANCED_FACE ( 'NONE', ( #15620, #3198 ), #8737, .T. ) ;
#4307 = FACE_OUTER_BOUND ( 'NONE', #9565, .T. ) ;
#4308 = DIRECTION ( 'NONE',  ( 1.000000000000000000, 0.000000000000000000, 0.000000000000000000 ) ) ;
#4309 = DIRECTION ( 'NONE',  ( 0.000000000000000000, 0.4999999999999991118, -0.8660254037844391517 ) ) ;
#4310 = CARTESIAN_POINT ( 'NONE',  ( 27.93049598394382116, -4.671775696577297410, 7.939653947423662039 ) ) ;
#4311 = DIRECTION ( 'NONE',  ( 0.1196152422706608098, -0.9928203230275511881, 0.000000000000000000 ) ) ;
#4312 = CARTESIAN_POINT ( 'NONE',  ( -13.65694651542706595, -25.37101204406941335, -16.45580752066269881 ) ) ;
#4313 = ADVANCED_FACE ( 'NONE', ( #10256 ), #17916, .T. ) ;
#4314 = CARTESIAN_POINT ( 'NONE',  ( 30.81132015408399027, -5.578634341498224458, 7.939653947423658487 ) ) ;
#4315 = ORIENTED_EDGE ( 'NONE', *, *, #4173, .T. ) ;
#4316 = CIRCLE ( 'NONE', #7810, 6.249999999999998224 ) ;
#4317 = ORIENTED_EDGE ( 'NONE', *, *, #17947, .F. ) ;
#4318 = ADVANCED_FACE ( 'NONE', ( #14531 ), #17170, .F. ) ;
#4319 = CARTESIAN_POINT ( 'NONE',  ( 26.86653773853314320, -2.919050055179571945, 4.705209693361167567 ) ) ;
#4320 = LINE ( 'NONE', #10106, #4956 ) ;
#4321 = DIRECTION ( 'NONE',  ( 0.000000000000000000, 1.000000000000000000, 0.000000000000000000 ) ) ;
#4322 = ORIENTED_EDGE ( 'NONE', *, *, #10769, .T. ) ;
#4323 = CARTESIAN_POINT ( 'NONE',  ( 28.08810621022444920, -4.652786776866828511, 7.939653947423662039 ) ) ;
#4324 = DIRECTION ( 'NONE',  ( 0.9928203230275512992, 0.1196152422706610180, 4.006172263299093133E-17 ) ) ;
#4325 = DIRECTION ( 'NONE',  ( 1.000000000000000000, 0.000000000000000000, 0.000000000000000000 ) ) ;
#4326 = CARTESIAN_POINT ( 'NONE',  ( 32.97211790677835097, -2.610546234160043610, -8.283357778048660691 ) ) ;
#4327 = CARTESIAN_POINT ( 'NONE',  ( 27.15566825608056689, -6.646038734597135011, -4.705209693361169343 ) ) ;
#4328 = CARTESIAN_POINT ( 'NONE',  ( 32.52441275490655670, -6.636378442139655220, -5.783357778048663356 ) ) ;
#4329 = CARTESIAN_POINT ( 'NONE',  ( 31.01321894478757812, -1.392741288986461212, -5.783357778048658027 ) ) ;
#4330 = EDGE_CURVE ( 'NONE', #1468, #15632, #7925, .T. ) ;
#4331 = DIRECTION ( 'NONE',  ( 1.000000000000000000, 0.000000000000000000, 0.000000000000000000 ) ) ;
#4332 = LINE ( 'NONE', #9844, #14772 ) ;
#4333 = CARTESIAN_POINT ( 'NONE',  ( 31.49429780130001433, -5.496349022752856861, -7.939653947423664704 ) ) ;
#4334 = ORIENTED_EDGE ( 'NONE', *, *, #2122, .T. ) ;
#4335 = CIRCLE ( 'NONE', #8972, 6.000000000000000888 ) ;
#4336 = CARTESIAN_POINT ( 'NONE',  ( 30.25524682244395436, -4.391689130744175884, -3.283357778048664688 ) ) ;
#4337 = ORIENTED_EDGE ( 'NONE', *, *, #1186, .T. ) ;
#4338 = AXIS2_PLACEMENT_3D ( 'NONE', #9112, #6387, #6114 ) ;
#4339 = ORIENTED_EDGE ( 'NONE', *, *, #5350, .T. ) ;
#4340 = ADVANCED_FACE ( 'NONE', ( #3368, #11970 ), #3550, .T. ) ;
#4341 = CARTESIAN_POINT ( 'NONE',  ( 28.86293393808771057, -2.678523738846987357, 6.861505862736165362 ) ) ;
#4342 = CARTESIAN_POINT ( 'NONE',  ( 32.83754810739938534, -9.116730809865837060, 15.78335777804866424 ) ) ;
#4343 = FACE_OUTER_BOUND ( 'NONE', #9828, .T. ) ;
#4344 = CIRCLE ( 'NONE', #8692, 2.000000000000001776 ) ;
#4345 = CARTESIAN_POINT ( 'NONE',  ( 25.95642634701329499, -4.403549397486640871, -3.686412874245495797 ) ) ;
#4346 = CARTESIAN_POINT ( 'NONE',  ( 32.87199790123699472, -1.558343308739095656, -5.783357778048663356 ) ) ;
#4347 = CARTESIAN_POINT ( 'NONE',  ( 28.75786045390062995, -2.691183018653962034, -6.861505862736159145 ) ) ;
#4348 = DIRECTION ( 'NONE',  ( -0.7681011886108269904, 0.5760758914581205481, 0.2795659695588259552 ) ) ;
#4349 = CARTESIAN_POINT ( 'NONE',  ( 20.00000000000000000, 7.999999999999996447, 12.00000000000000000 ) ) ;
#4350 = ORIENTED_EDGE ( 'NONE', *, *, #2408, .F. ) ;
#4351 = CARTESIAN_POINT ( 'NONE',  ( 34.43754810739937966, -7.916730809865828888, 5.783357778048663356 ) ) ;
#4352 =( GEOMETRIC_REPRESENTATION_CONTEXT ( 3 ) GLOBAL_UNCERTAINTY_ASSIGNED_CONTEXT ( ( #279 ) ) GLOBAL_UNIT_ASSIGNED_CONTEXT ( ( #1494, #5731, #9806 ) ) REPRESENTATION_CONTEXT ( 'NONE', 'WORKASPACE' ) );
#4353 = CARTESIAN_POINT ( 'NONE',  ( 28.64916707261694384, -6.765910400363817523, -4.533357778048668685 ) ) ;
#4354 = AXIS2_PLACEMENT_3D ( 'NONE', #7777, #11754, #17324 ) ;
#4355 = CARTESIAN_POINT ( 'NONE',  ( 30.25080928106424594, -3.138282701210941994, -3.627061608673662896 ) ) ;
#4356 = DIRECTION ( 'NONE',  ( -1.000000000000000000, 0.000000000000000000, 0.000000000000000000 ) ) ;
#4357 = LINE ( 'NONE', #9601, #10898 ) ;
#4358 = CARTESIAN_POINT ( 'NONE',  ( 5.499998817156068753, -20.49639288455253450, -13.00000000000000178 ) ) ;
#4359 = VERTEX_POINT ( 'NONE', #7543 ) ;
#4360 = CARTESIAN_POINT ( 'NONE',  ( -5.560781378645573980, 0.000000000000000000, -3.700000000000000178 ) ) ;
#4361 = AXIS2_PLACEMENT_3D ( 'NONE', #4349, #7260, #13963 ) ;
#4362 = CARTESIAN_POINT ( 'NONE',  ( 30.61177514885987350, -5.802548093181622235, 3.283357778048663800 ) ) ;
#4363 = CARTESIAN_POINT ( 'NONE',  ( 29.62489513447700062, -6.348545659133139729, -6.861505862736166250 ) ) ;
#4364 = EDGE_LOOP ( 'NONE', ( #16809, #4302, #2960, #5847, #11879 ) ) ;
#4365 = EDGE_CURVE ( 'NONE', #17122, #3121, #9743, .T. ) ;
#4366 = AXIS2_PLACEMENT_3D ( 'NONE', #13163, #4633, #3372 ) ;
#4367 = ORIENTED_EDGE ( 'NONE', *, *, #6271, .F. ) ;
#4368 = CARTESIAN_POINT ( 'NONE',  ( 38.64694918415791136, -1.054552983374777986, -9.783357778048662468 ) ) ;
#4369 = DIRECTION ( 'NONE',  ( 1.000000000000000000, 0.000000000000000000, 0.000000000000000000 ) ) ;
#4370 = CYLINDRICAL_SURFACE ( 'NONE', #15365, 5.000000000000000000 ) ;
#4371 = ORIENTED_EDGE ( 'NONE', *, *, #14666, .F. ) ;
#4372 =( REPRESENTATION_RELATIONSHIP ('NONE','NONE', #3227, #1480 ) REPRESENTATION_RELATIONSHIP_WITH_TRANSFORMATION ( #17209 )SHAPE_REPRESENTATION_RELATIONSHIP( ) );
#4373 = CIRCLE ( 'NONE', #17735, 13.00000000000000178 ) ;
#4374 = DIRECTION ( 'NONE',  ( -0.000000000000000000, -0.000000000000000000, 1.000000000000000000 ) ) ;
#4375 = VERTEX_POINT ( 'NONE', #11783 ) ;
#4376 = VERTEX_POINT ( 'NONE', #4896 ) ;
#4377 = CARTESIAN_POINT ( 'NONE',  ( 32.14665875496697822, -6.044722943765660439, -6.861505862736166250 ) ) ;
#4378 = CARTESIAN_POINT ( 'NONE',  ( 4.000000000000000000, 1.658584703716865061, -3.231554742509319844 ) ) ;
#4379 = CIRCLE ( 'NONE', #16830, 10.50000000000000000 ) ;
#4380 = CARTESIAN_POINT ( 'NONE',  ( 31.94023320572814484, -7.096308717197083560, -5.783357778048669573 ) ) ;
#4381 = CARTESIAN_POINT ( 'NONE',  ( 28.48706592061337162, -2.086641016831144668, 6.453230759126468818 ) ) ;
#4382 = ORIENTED_EDGE ( 'NONE', *, *, #6273, .F. ) ;
#4383 = CARTESIAN_POINT ( 'NONE',  ( 32.34358231980129261, -4.140085944684206432, 7.939653947423662039 ) ) ;
#4384 = VECTOR ( 'NONE', #2229, 1000.000000000000000 ) ;
#4385 = EDGE_CURVE ( 'NONE', #1595, #12357, #7637, .T. ) ;
#4386 = CARTESIAN_POINT ( 'NONE',  ( 27.14244485254070938, -4.766720295129625029, 3.627061608673664228 ) ) ;
#4387 = CARTESIAN_POINT ( 'NONE',  ( -21.42418507870700850, -22.26964835135415655, 15.24537475165205791 ) ) ;
#4388 = ORIENTED_EDGE ( 'NONE', *, *, #15775, .F. ) ;
#4389 = AXIS2_PLACEMENT_3D ( 'NONE', #13172, #4908, #931 ) ;
#4390 = FILL_AREA_STYLE_COLOUR ( '', #11954 ) ;
#4391 = EDGE_LOOP ( 'NONE', ( #11757, #4743, #516, #13221, #5306, #584 ) ) ;
#4392 = CARTESIAN_POINT ( 'NONE',  ( 9.099998387031005720, -19.29508120620799971, 6.000000000000000000 ) ) ;
#4393 = EDGE_LOOP ( 'NONE', ( #8466, #15017, #11576, #7109, #5872 ) ) ;
#4394 = EDGE_CURVE ( 'NONE', #3955, #16943, #17540, .T. ) ;
#4395 = CARTESIAN_POINT ( 'NONE',  ( 25.88156304229571703, -4.918631652813365562, -7.939653947423662039 ) ) ;
#4396 = AXIS2_PLACEMENT_3D ( 'NONE', #13366, #16277, #6481 ) ;
#4397 = CARTESIAN_POINT ( 'NONE',  ( 31.20090818012769773, -4.277755612481361602, -8.283357778048662468 ) ) ;
#4398 = CARTESIAN_POINT ( 'NONE',  ( 28.11132641904908169, -7.168068194032743534, 5.783357778048657138 ) ) ;
#4399 = APPLICATION_PROTOCOL_DEFINITION ( 'draft international standard', 'automotive_design', 1998, #12677 ) ;
#4400 = CYLINDRICAL_SURFACE ( 'NONE', #8670, 2.749999999999992006 ) ;
#4401 = CARTESIAN_POINT ( 'NONE',  ( 32.92264866086529906, -1.552240892477451339, -6.453230759126466154 ) ) ;
#4402 = CARTESIAN_POINT ( 'NONE',  ( 27.87986455999572399, -6.131689368163070419, -3.283357778048667797 ) ) ;
#4403 = LINE ( 'NONE', #9918, #15892 ) ;
#4404 = CARTESIAN_POINT ( 'NONE',  ( 31.04338717100262102, -6.177645381738930297, 4.705209693361159573 ) ) ;
#4405 = ORIENTED_EDGE ( 'NONE', *, *, #6625, .F. ) ;
#4406 = VECTOR ( 'NONE', #773, 1000.000000000000227 ) ;
#4407 = TOROIDAL_SURFACE ( 'NONE', #16565, 12.70000000000000284, 0.9000000000000003553 ) ;
#4408 = EDGE_CURVE ( 'NONE', #3520, #16322, #1090, .T. ) ;
#4409 = ORIENTED_EDGE ( 'NONE', *, *, #11476, .F. ) ;
#4410 = CARTESIAN_POINT ( 'NONE',  ( 27.50150540219088313, -5.977401655418042914, 7.939653947423658487 ) ) ;
#4411 = DIRECTION ( 'NONE',  ( 0.9928203230275512992, 0.1196152422706614898, -0.000000000000000000 ) ) ;
#4412 = DIRECTION ( 'NONE',  ( 0.000000000000000000, 1.000000000000000000, 3.469446951953614189E-16 ) ) ;
#4413 = VERTEX_POINT ( 'NONE', #4719 ) ;
#4414 = CARTESIAN_POINT ( 'NONE',  ( 25.99533317148741318, -3.650983533393564517, 7.939653947423662927 ) ) ;
#4415 = CARTESIAN_POINT ( 'NONE',  ( -8.632250723006720250, -18.84644399697197770, 13.00000000000000178 ) ) ;
#4416 = CARTESIAN_POINT ( 'NONE',  ( 38.02246887229409111, 4.128705714927905390, 0.2592325134722451851 ) ) ;
#4417 = CARTESIAN_POINT ( 'NONE',  ( 33.26181313012506280, -6.547536259434060923, -6.453230759126471483 ) ) ;
#4419 = AXIS2_PLACEMENT_3D ( 'NONE', #6309, #3410, #5033 ) ;
#4418 = DIRECTION ( 'NONE',  ( -1.000000000000000000, -0.000000000000000000, -0.000000000000000000 ) ) ;
#4420 = FACE_OUTER_BOUND ( 'NONE', #893, .T. ) ;
#4421 = ADVANCED_FACE ( 'NONE', ( #2204 ), #7717, .F. ) ;
#4422 = CARTESIAN_POINT ( 'NONE',  ( 33.17547354829333273, -5.293800545841212291, -3.627061608673667781 ) ) ;
#4423 = COLOUR_RGB ( '', 0.66274510, 0.83137255, 0.94901961) ;
#4424 = DIRECTION ( 'NONE',  ( 0.000000000000000000, 0.000000000000000000, 1.000000000000000000 ) ) ;
#4425 = CARTESIAN_POINT ( 'NONE',  ( 3.248936832696172505, -15.16081378324841289, 17.00000000000000000 ) ) ;
#4426 = CARTESIAN_POINT ( 'NONE',  ( 31.91006497951310550, -2.311404624444611589, -6.861505862736159145 ) ) ;
#4427 = VERTEX_POINT ( 'NONE', #10244 ) ;
#4428 = AXIS2_PLACEMENT_3D ( 'NONE', #6300, #15919, #3494 ) ;
#4429 =( BOUNDED_CURVE ( )  B_SPLINE_CURVE ( 2, ( #2790, #4658, #15819, #7478, #15637, #9742, #6955, #416, #5921 ),
 .UNSPECIFIED., .F., .T. ) 
 B_SPLINE_CURVE_WITH_KNOTS ( ( 3, 2, 2, 2, 3 ),
 ( 0.9038461538461538547, 0.9102564102564102422, 0.9230769230769231282, 0.9358974358974359031, 0.9423076923076922906 ),
 .UNSPECIFIED. ) 
 CURVE ( )  GEOMETRIC_REPRESENTATION_ITEM ( )  RATIONAL_B_SPLINE_CURVE ( ( 0.9330127018922194093, 0.9330127018922194093, 1.000000000000000000, 0.8660254037844387076, 1.000000000000000000, 0.8660254037844387076, 1.000000000000000000, 0.9330127018922194093, 0.9330127018922194093 ) ) 
 REPRESENTATION_ITEM ( '' )  );
#4430 = CARTESIAN_POINT ( 'NONE',  ( 15.92260893619738837, -28.39189527176317540, 16.15082599432113142 ) ) ;
#4431 = CARTESIAN_POINT ( 'NONE',  ( 30.71189515440122975, -6.854751018602581958, -5.783357778048663356 ) ) ;
#4432 = CIRCLE ( 'NONE', #11963, 10.50000000000000000 ) ;
#4433 = EDGE_LOOP ( 'NONE', ( #12591, #16245 ) ) ;
#4434 = ORIENTED_EDGE ( 'NONE', *, *, #11592, .F. ) ;
#4435 = CARTESIAN_POINT ( 'NONE',  ( 28.88938074516742205, -6.437160617781993999, 6.861505862736158257 ) ) ;
#4436 = AXIS2_PLACEMENT_3D ( 'NONE', #4368, #14155, #12701 ) ;
#4437 = CARTESIAN_POINT ( 'NONE',  ( 26.47269060886452507, -6.728324053342490174, -6.861505862736166250 ) ) ;
#4438 = PLANE ( 'NONE',  #15878 ) ;
#4439 = CARTESIAN_POINT ( 'NONE',  ( -35.77680296528374271, -19.03270077640483038, -0.5379818257722512875 ) ) ;
#4440 = DIRECTION ( 'NONE',  ( 0.6000000000000000888, 0.7999999999999999334, -0.000000000000000000 ) ) ;
#4441 = CARTESIAN_POINT ( 'NONE',  ( 31.65190802758064592, -5.477360103042387074, -7.939653947423664704 ) ) ;
#4442 = CARTESIAN_POINT ( 'NONE',  ( -2.687328764639636880, 3.067272167851287534, -0.05923475698270543044 ) ) ;
#4443 = DIRECTION ( 'NONE',  ( 0.000000000000000000, 0.000000000000000000, 1.000000000000000000 ) ) ;
#4444 = CARTESIAN_POINT ( 'NONE',  ( -2.016448651773435938E-27, -20.49999999999999645, -13.00000000000000178 ) ) ;
#4445 = UNCERTAINTY_MEASURE_WITH_UNIT (LENGTH_MEASURE( 1.000000000000000082E-05 ), #13509, 'distance_accuracy_value', 'NONE');
#4446 = CARTESIAN_POINT ( 'NONE',  ( -9.647391702364178201, 16.07861560120820243, 16.78732711007196698 ) ) ;
#4447 = ORIENTED_EDGE ( 'NONE', *, *, #3072, .F. ) ;
#4448 = EDGE_CURVE ( 'NONE', #4167, #1847, #15792, .T. ) ;
#4449 = CARTESIAN_POINT ( 'NONE',  ( 29.50659824675005893, -4.481886499472614638, -7.939653947423662039 ) ) ;
#4450 = DIRECTION ( 'NONE',  ( 0.7071067811865489050, 0.000000000000000000, 0.7071067811865462405 ) ) ;
#4451 = DIRECTION ( 'NONE',  ( 0.000000000000000000, -1.000000000000000000, 0.000000000000000000 ) ) ;
#4452 = CARTESIAN_POINT ( 'NONE',  ( -29.25000000000000000, -16.21813761408365195, 13.00000000000000178 ) ) ;
#4453 = CARTESIAN_POINT ( 'NONE',  ( 27.85662501549087366, -2.162596695673018043, 6.453230759126474148 ) ) ;
#4454 = CARTESIAN_POINT ( 'NONE',  ( 30.17644170758179101, -4.401183590806859947, 8.283357778048662468 ) ) ;
#4455 = CARTESIAN_POINT ( 'NONE',  ( 25.99795558426325215, -4.648046406214923820, -3.627061608673664228 ) ) ;
#4456 = ORIENTED_EDGE ( 'NONE', *, *, #17544, .F. ) ;
#4457 = CARTESIAN_POINT ( 'NONE',  ( 25.71748644841968456, -2.420320648352051851, -5.783357778048663356 ) ) ;
#4458 = DIRECTION ( 'NONE',  ( -0.000000000000000000, -0.000000000000000000, -1.000000000000000000 ) ) ;
#4459 = CARTESIAN_POINT ( 'NONE',  ( 45.50000000000000000, -19.03270077640483038, 5.537981825772250843 ) ) ;
#4460 = ORIENTED_EDGE ( 'NONE', *, *, #9181, .F. ) ;
#4461 = CARTESIAN_POINT ( 'NONE',  ( 26.39823381822652593, -6.110324093391315436, -3.627061608673668225 ) ) ;
#4462 = EDGE_CURVE ( 'NONE', #63, #13752, #2935, .T. ) ;
#4463 = CARTESIAN_POINT ( 'NONE',  ( 31.39792096211754924, -4.254019462947003838, -7.939653947423662039 ) ) ;
#4464 = ADVANCED_FACE ( 'NONE', ( #3346 ), #3523, .F. ) ;
#4465 = CARTESIAN_POINT ( 'NONE',  ( 27.82847066025702887, -2.165988739474055791, -5.783357778048658027 ) ) ;
#4466 = LINE ( 'NONE', #14079, #567 ) ;
#4467 = CARTESIAN_POINT ( 'NONE',  ( -14.00000000000000178, 0.000000000000000000, 10.50000000000000000 ) ) ;
#4468 = ORIENTED_EDGE ( 'NONE', *, *, #10158, .T. ) ;
#4469 = CARTESIAN_POINT ( 'NONE',  ( 32.33415724766913257, -1.960501102408027219, -4.533357778048659803 ) ) ;
#4470 = DIRECTION ( 'NONE',  ( -0.000000000000000000, -0.000000000000000000, -1.000000000000000000 ) ) ;
#4471 = ORIENTED_EDGE ( 'NONE', *, *, #12646, .F. ) ;
#4472 = CARTESIAN_POINT ( 'NONE',  ( 32.02836186724004364, -4.178063784105134459, 3.627061608673664228 ) ) ;
#4473 =( REPRESENTATION_RELATIONSHIP ('NONE','NONE', #3227, #12598 ) REPRESENTATION_RELATIONSHIP_WITH_TRANSFORMATION ( #12001 )SHAPE_REPRESENTATION_RELATIONSHIP( ) );
#4474 = CARTESIAN_POINT ( 'NONE',  ( 27.78610916120306129, -6.570083055755264745, 6.861505862736157368 ) ) ;
#4475 = CARTESIAN_POINT ( 'NONE',  ( -18.90235488073503944, -20.95521764957430122, 15.70196361584510392 ) ) ;
#4476 = DIRECTION ( 'NONE',  ( 0.000000000000000000, 0.000000000000000000, -1.000000000000000000 ) ) ;
#4477 = EDGE_LOOP ( 'NONE', ( #17425, #13350 ) ) ;
#4478 = CARTESIAN_POINT ( 'NONE',  ( 30.98067518586950442, -1.786210345264705790, 5.783357778048667797 ) ) ;
#4479 = ORIENTED_EDGE ( 'NONE', *, *, #3415, .T. ) ;
#4480 = LINE ( 'NONE', #8475, #13324 ) ;
#4481 = ORIENTED_EDGE ( 'NONE', *, *, #5277, .F. ) ;
#4482 = DIRECTION ( 'NONE',  ( -0.9928203230275511881, -0.1196152422706614482, -0.000000000000000000 ) ) ;
#4483 = CARTESIAN_POINT ( 'NONE',  ( 26.82722439997946395, -4.804698134550569044, -3.627061608673664672 ) ) ;
#4484 = EDGE_CURVE ( 'NONE', #13130, #1572, #5053, .T. ) ;
#4485 = CARTESIAN_POINT ( 'NONE',  ( 33.18226487515251222, -2.585227674546096033, -3.283357778048662023 ) ) ;
#4486 = DIRECTION ( 'NONE',  ( -0.9928203230275512992, -0.1196152422706610319, -9.614813431917826478E-17 ) ) ;
#4487 = CONTEXT_DEPENDENT_SHAPE_REPRESENTATION ( #6197, #6507 ) ;
#4488 = CARTESIAN_POINT ( 'NONE',  ( -20.25000000000001066, -16.21813761408365195, 13.00000000000000355 ) ) ;
#4489 = CARTESIAN_POINT ( 'NONE',  ( 28.91547068018125799, -2.672194098943493135, -6.861505862736158257 ) ) ;
#4490 = CARTESIAN_POINT ( 'NONE',  ( -4.197393957002304887, -0.8151795401431392030, -3.203767560748937537 ) ) ;
#4491 = FACE_OUTER_BOUND ( 'NONE', #10765, .T. ) ;
#4492 = LINE ( 'NONE', #11169, #10065 ) ;
#4493 = CARTESIAN_POINT ( 'NONE',  ( 31.69574812466957781, -6.726019302751734763, 5.783357778048657138 ) ) ;
#4494 = ORIENTED_EDGE ( 'NONE', *, *, #9496, .F. ) ;
#4495 = CARTESIAN_POINT ( 'NONE',  ( -10.47816170930907553, 0.6768509389586230274, -7.794427190999915211 ) ) ;
#4496 = VERTEX_POINT ( 'NONE', #11760 ) ;
#4497 = CARTESIAN_POINT ( 'NONE',  ( 29.51982165028991645, -6.361204938940122844, 6.861505862736158257 ) ) ;
#4498 = DIRECTION ( 'NONE',  ( -0.000000000000000000, -0.000000000000000000, -1.000000000000000000 ) ) ;
#4499 = FACE_OUTER_BOUND ( 'NONE', #12923, .T. ) ;
#4500 = ORIENTED_EDGE ( 'NONE', *, *, #8547, .T. ) ;
#4501 = CARTESIAN_POINT ( 'NONE',  ( 26.65222088368961195, -7.333664733486695120, 5.783357778048657138 ) ) ;
#4502 = VERTEX_POINT ( 'NONE', #12950 ) ;
#4503 = FACE_OUTER_BOUND ( 'NONE', #7765, .T. ) ;
#4505 = CARTESIAN_POINT ( 'NONE',  ( -45.50000000000000000, -16.03270077640482683, -5.537981825772250843 ) ) ;
#4504 = AXIS2_PLACEMENT_3D ( 'NONE', #13743, #4138, #2594 ) ;
#4506 = CARTESIAN_POINT ( 'NONE',  ( 8.409399735147209713E-16, 4.618802153517009401, -3.204269196027528022 ) ) ;
#4507 = FACE_BOUND ( 'NONE', #3257, .T. ) ;
#4508 = CARTESIAN_POINT ( 'NONE',  ( 27.57216386142120257, -6.895668018177890879, -7.033357778048666908 ) ) ;
#4509 = CARTESIAN_POINT ( 'NONE',  ( -11.80000000000000249, 0.000000000000000000, 1.102182119232619020E-16 ) ) ;
#4510 = CARTESIAN_POINT ( 'NONE',  ( -2.500000000000000888, 3.061616997868384127E-16, -25.03750572909317285 ) ) ;
#4511 = CARTESIAN_POINT ( 'NONE',  ( 32.54503264317084188, -5.369756224683081669, -3.627061608673667781 ) ) ;
#4512 = EDGE_CURVE ( 'NONE', #6446, #4895, #894, .T. ) ;
#4513 = CARTESIAN_POINT ( 'NONE',  ( 28.82057243903374655, -7.082618055128190093, 5.783357778048657138 ) ) ;
#4514 = CARTESIAN_POINT ( 'NONE',  ( 27.38828526237195504, -6.917821758047558056, -4.533357778048668685 ) ) ;
#4515 = ORIENTED_EDGE ( 'NONE', *, *, #1512, .F. ) ;
#4516 = EDGE_CURVE ( 'NONE', #16863, #16943, #3433, .T. ) ;
#4517 = VERTEX_POINT ( 'NONE', #17432 ) ;
#4518 = VERTEX_POINT ( 'NONE', #8878 ) ;
#4519 = CARTESIAN_POINT ( 'NONE',  ( 28.98992747081926069, -3.290194058894681639, 7.939653947423662927 ) ) ;
#4520 = CARTESIAN_POINT ( 'NONE',  ( 26.66961417369883591, -4.823687054261037055, -3.627061608673664672 ) ) ;
#4521 = CARTESIAN_POINT ( 'NONE',  ( 26.31065902414478686, -7.328232685206446106, 5.254681170202263552 ) ) ;
#4522 = LINE ( 'NONE', #14136, #10396 ) ;
#4523 = DIRECTION ( 'NONE',  ( 0.9928203230275510771, 0.1196152422706609902, 4.006172263299092517E-17 ) ) ;
#4524 = CARTESIAN_POINT ( 'NONE',  ( 31.44176105920648823, -5.502678662656354192, -3.627061608673668225 ) ) ;
#4525 = CARTESIAN_POINT ( 'NONE',  ( 2.749999999999992895, -20.49999999999999645, -13.00000000000000178 ) ) ;
#4526 = LINE ( 'NONE', #6058, #9290 ) ;
#4527 = DIRECTION ( 'NONE',  ( 0.000000000000000000, 0.000000000000000000, 1.000000000000000000 ) ) ;
#4528 = CARTESIAN_POINT ( 'NONE',  ( 26.30185955129047315, -7.986322017489088765, -6.648778972250404706 ) ) ;
#4529 = EDGE_CURVE ( 'NONE', #14120, #11482, #8962, .T. ) ;
#4530 = CARTESIAN_POINT ( 'NONE',  ( 31.39792096211754924, -4.254019462947003838, -7.939653947423662039 ) ) ;
#4531 = DIRECTION ( 'NONE',  ( 1.000000000000000000, 0.000000000000000000, 0.000000000000000000 ) ) ;
#4532 = CARTESIAN_POINT ( 'NONE',  ( 26.24651417059167358, -6.811311830135031720, -4.396611942026659392 ) ) ;
#4533 = EDGE_LOOP ( 'NONE', ( #798, #2361, #8415, #13671 ) ) ;
#4534 = CARTESIAN_POINT ( 'NONE',  ( 0.000000000000000000, 0.000000000000000000, -2.000000000000000000 ) ) ;
#4535 = CARTESIAN_POINT ( 'NONE',  ( 27.87986455999572399, -6.131689368163069531, 8.283357778048658915 ) ) ;
#4536 = CARTESIAN_POINT ( 'NONE',  ( 26.21417678486618641, -2.370676134166772808, -5.783357778048658915 ) ) ;
#4537 = VERTEX_POINT ( 'NONE', #14506 ) ;
#4538 = CARTESIAN_POINT ( 'NONE',  ( 33.40301380667672504, -2.758504307001591993, -3.627061608673662896 ) ) ;
#4539 = ORIENTED_EDGE ( 'NONE', *, *, #3039, .F. ) ;
#4540 = EDGE_CURVE ( 'NONE', #17902, #5885, #6643, .T. ) ;
#4541 = CARTESIAN_POINT ( 'NONE',  ( -25.20502126318114833, -10.36657009486825842, -14.42817146764052083 ) ) ;
#4542 = EDGE_LOOP ( 'NONE', ( #7276, #115, #15794, #10722 ) ) ;
#4543 = VECTOR ( 'NONE', #8436, 1000.000000000000227 ) ;
#4544 = ORIENTED_EDGE ( 'NONE', *, *, #13626, .T. ) ;
#4545 = CARTESIAN_POINT ( 'NONE',  ( 26.52522735095806894, -6.721994413439005278, -4.705209693361169343 ) ) ;
#4546 = VECTOR ( 'NONE', #15808, 1000.000000000000000 ) ;
#4547 = ORIENTED_EDGE ( 'NONE', *, *, #3938, .T. ) ;
#4548 = CARTESIAN_POINT ( 'NONE',  ( 30.12381574833269937, -2.526612381163247267, -4.705209693361161349 ) ) ;
#4549 = CARTESIAN_POINT ( 'NONE',  ( 26.13613979636700080, -5.895191778948487560, 5.783357778048662468 ) ) ;
#4550 = DIRECTION ( 'NONE',  ( 0.9928203230275510771, 0.1196152422706614621, -0.000000000000000000 ) ) ;
#4551 = CARTESIAN_POINT ( 'NONE',  ( -2.016448651773435938E-27, -20.49999999999999645, 6.000000000000000000 ) ) ;
#4552 = CARTESIAN_POINT ( 'NONE',  ( 32.92339180097568629, -5.524043937428110063, -3.283357778048667797 ) ) ;
#4553 = DIRECTION ( 'NONE',  ( -0.7999999999999999334, 0.6000000000000000888, 0.000000000000000000 ) ) ;
#4554 = CARTESIAN_POINT ( 'NONE',  ( 25.63782166807609997, -6.407846580969937200, 3.746366521588336163 ) ) ;
#4555 = CONICAL_SURFACE ( 'NONE', #1368, 9.500000000000001776, 0.7853981633974465026 ) ;
#4556 = EDGE_CURVE ( 'NONE', #10267, #15625, #16054, .T. ) ;
#4557 = CARTESIAN_POINT ( 'NONE',  ( 8.472608240843633681E-22, -7.722472891792491889E-22, -7.794427190999915211 ) ) ;
#4558 = CARTESIAN_POINT ( 'NONE',  ( -23.83685604381143364, -22.42490655540755284, 14.74319968589249719 ) ) ;
#4559 = DIRECTION ( 'NONE',  ( 0.000000000000000000, 0.000000000000000000, -1.000000000000000000 ) ) ;
#4560 = VERTEX_POINT ( 'NONE', #14604 ) ;
#4561 = CARTESIAN_POINT ( 'NONE',  ( 26.18940839444933033, -6.337336286969802224, -7.823481096485427777 ) ) ;
#4562 = ORIENTED_EDGE ( 'NONE', *, *, #2762, .T. ) ;
#4563 = DIRECTION ( 'NONE',  ( -0.000000000000000000, -0.000000000000000000, -1.000000000000000000 ) ) ;
#4564 = CARTESIAN_POINT ( 'NONE',  ( -23.02601376483258022, 3.965314980223224151, 0.000000000000000000 ) ) ;
#4565 = ORIENTED_EDGE ( 'NONE', *, *, #1194, .T. ) ;
#4566 = ORIENTED_EDGE ( 'NONE', *, *, #11072, .F. ) ;
#4567 = CARTESIAN_POINT ( 'NONE',  ( 26.64639396487419987, -2.308405637095112706, -5.783357778048658027 ) ) ;
#4568 = CARTESIAN_POINT ( 'NONE',  ( 27.65458886993626564, -2.824105456627233224, -6.861505862736158257 ) ) ;
#4569 = CARTESIAN_POINT ( 'NONE',  ( 32.77701044293393551, -4.087866415376695706, -3.283357778048664688 ) ) ;
#4570 = CARTESIAN_POINT ( 'NONE',  ( 45.50000000000000000, -19.03270077640483038, 8.287981825772241962 ) ) ;
#4571 = ADVANCED_FACE ( 'NONE', ( #2182 ), #8501, .F. ) ;
#4572 =( NAMED_UNIT ( * ) SI_UNIT ( $, .STERADIAN. ) SOLID_ANGLE_UNIT ( ) );
#4573 = FACE_OUTER_BOUND ( 'NONE', #3714, .T. ) ;
#4574 = CARTESIAN_POINT ( 'NONE',  ( 28.40332666278570173, -4.614808937445885384, -7.939653947423662039 ) ) ;
#4575 = FACE_OUTER_BOUND ( 'NONE', #9715, .T. ) ;
#4576 = CARTESIAN_POINT ( 'NONE',  ( 46.37688276194213444, -2.449350377220338881, -5.783357778048662468 ) ) ;
#4577 = CARTESIAN_POINT ( 'NONE',  ( -9.099998387031003944, -19.29508120620799616, -16.81964500401478091 ) ) ;
#4578 = CARTESIAN_POINT ( 'NONE',  ( 28.91999743871649997, -5.806501378023834370, 7.939653947423658487 ) ) ;
#4579 = ORIENTED_EDGE ( 'NONE', *, *, #14326, .T. ) ;
#4580 = CARTESIAN_POINT ( 'NONE',  ( 27.10313151398701947, -6.652368374500619908, -6.861505862736166250 ) ) ;
#4581 = ORIENTED_EDGE ( 'NONE', *, *, #6190, .T. ) ;
#4582 = EDGE_CURVE ( 'NONE', #11951, #9378, #9200, .T. ) ;
#4583 = CARTESIAN_POINT ( 'NONE',  ( 31.45915434921569798, -2.992700983430681028, 3.627061608673666893 ) ) ;
#4584 = CARTESIAN_POINT ( 'NONE',  ( 32.60321786976872005, -6.626883982076972934, -5.783357778048663356 ) ) ;
#4585 = CYLINDRICAL_SURFACE ( 'NONE', #7601, 2.500000000000001776 ) ;
#4586 = VERTEX_POINT ( 'NONE', #4211 ) ;
#4587 = CARTESIAN_POINT ( 'NONE',  ( 3.999999999999998224, 0.000000000000000000, 0.000000000000000000 ) ) ;
#4588 = AXIS2_PLACEMENT_3D ( 'NONE', #17109, #3313, #11449 ) ;
#4589 = CARTESIAN_POINT ( 'NONE',  ( -4.203934431905299363, -1.640681339110445114, -3.298434044919825503 ) ) ;
#4590 = EDGE_LOOP ( 'NONE', ( #10956, #3188 ) ) ;
#4591 = CARTESIAN_POINT ( 'NONE',  ( 13.00000000000000178, 0.000000000000000000, -10.50000000000000000 ) ) ;
#4592 = DIRECTION ( 'NONE',  ( 0.000000000000000000, 0.000000000000000000, -1.000000000000000000 ) ) ;
#4593 = VERTEX_POINT ( 'NONE', #9713 ) ;
#4594 = CARTESIAN_POINT ( 'NONE',  ( 26.63392073224175505, -2.647267031729148012, -7.033357778048658027 ) ) ;
#4595 = CARTESIAN_POINT ( 'NONE',  ( 32.52441275490655670, -6.636378442139655220, -5.783357778048663356 ) ) ;
#4596 = LINE ( 'NONE', #1811, #5006 ) ;
#4597 = CARTESIAN_POINT ( 'NONE',  ( 30.78070346053490880, -6.209293581256383199, -4.705209693361168455 ) ) ;
#4598 = ORIENTED_EDGE ( 'NONE', *, *, #6536, .F. ) ;
#4599 = CARTESIAN_POINT ( 'NONE',  ( 26.19678349485696955, -4.880653813392439311, -3.627061608673664672 ) ) ;
#4600 = CARTESIAN_POINT ( 'NONE',  ( 33.00219691583784964, -5.514549477365426888, 8.283357778048658915 ) ) ;
#4601 = AXIS2_PLACEMENT_3D ( 'NONE', #2371, #13507, #7889 ) ;
#4602 = EDGE_LOOP ( 'NONE', ( #16336, #10291, #3071, #10243, #5181, #16385, #11330, #9461, #16526 ) ) ;
#4603 = ORIENTED_EDGE ( 'NONE', *, *, #9645, .F. ) ;
#4604 = ORIENTED_EDGE ( 'NONE', *, *, #8554, .F. ) ;
#4605 = CARTESIAN_POINT ( 'NONE',  ( 28.77978050244509944, -3.315512618508630549, 3.627061608673666449 ) ) ;
#4606 = VECTOR ( 'NONE', #4664, 1000.000000000000000 ) ;
#4607 = CARTESIAN_POINT ( 'NONE',  ( 31.66250999073069750, -5.675955295111850596, 8.283357778048660691 ) ) ;
#4608 = FACE_OUTER_BOUND ( 'NONE', #1403, .T. ) ;
#4609 = EDGE_CURVE ( 'NONE', #15022, #2542, #17038, .T. ) ;
#4610 = DIRECTION ( 'NONE',  ( -1.000000000000000000, 0.000000000000000000, 0.000000000000000000 ) ) ;
#4611 = CARTESIAN_POINT ( 'NONE',  ( -23.47400307746860548, -29.47066586337336247, 14.90105725137467552 ) ) ;
#4612 = CARTESIAN_POINT ( 'NONE',  ( 33.30663696749426350, -1.516174747195733863, -5.783357778048658027 ) ) ;
#4613 = DIRECTION ( 'NONE',  ( 1.000000000000000000, 0.000000000000000000, 0.000000000000000000 ) ) ;
#4614 = CIRCLE ( 'NONE', #13015, 13.00000000000000178 ) ;
#4615 = CARTESIAN_POINT ( 'NONE',  ( 4.906836669863238853, 17.52808241874658890, 16.98904569177533119 ) ) ;
#4616 = CARTESIAN_POINT ( 'NONE',  ( 27.50829672905005907, -3.268828784122926212, -3.283357778048662023 ) ) ;
#4617 = CARTESIAN_POINT ( 'NONE',  ( -11.90182750357594621, 14.98910623166845646, 16.60584412753037853 ) ) ;
#4618 = B_SPLINE_CURVE_WITH_KNOTS ( 'NONE', 3,
 ( #3567, #16173, #7728, #10436, #17469, #2215, #11982, #3918, #12062, #17649, #5259, #9349, #13255, #14887, #14634, #6275, #14969, #17565 ),
 .UNSPECIFIED., .F., .F.,
 ( 4, 2, 2, 2, 2, 2, 2, 2, 4 ),
 ( 0.000000000000000000, 0.0005710890023745246154, 0.001142178004749049231, 0.001713267007123573955, 0.002284356009498098462, 0.002855445011872622969, 0.003426534014247147909, 0.003997623016621672416, 0.004568712018996196923 ),
 .UNSPECIFIED. ) ;
#4619 = VERTEX_POINT ( 'NONE', #11073 ) ;
#4620 = CARTESIAN_POINT ( 'NONE',  ( 28.38593337277646711, -7.124786616671554107, -5.783357778048668685 ) ) ;
#4621 = CARTESIAN_POINT ( 'NONE',  ( 30.66050125466253107, -2.889050389913576655, -3.283357778048662023 ) ) ;
#4622 = CARTESIAN_POINT ( 'NONE',  ( 26.86291784143654127, -6.981118157082444320, -7.033357778048666908 ) ) ;
#4623 = CARTESIAN_POINT ( 'NONE',  ( 50.00000000000000000, -16.03270077640482683, 5.537981825772250843 ) ) ;
#4624 = CIRCLE ( 'NONE', #6935, 25.00000000000000000 ) ;
#4625 = LINE ( 'NONE', #16793, #6902 ) ;
#4626 = CARTESIAN_POINT ( 'NONE',  ( 27.38828526237195504, -6.917821758047558056, 7.033357778048657138 ) ) ;
#4627 = CARTESIAN_POINT ( 'NONE',  ( 26.99805802979993885, -6.665027654307603022, -4.705209693361168455 ) ) ;
#4628 = AXIS2_PLACEMENT_3D ( 'NONE', #17856, #2768, #5376 ) ;
#4629 = ORIENTED_EDGE ( 'NONE', *, *, #14838, .F. ) ;
#4630 = PLANE ( 'NONE',  #16310 ) ;
#4631 = ORIENTED_EDGE ( 'NONE', *, *, #15161, .F. ) ;
#4632 = EDGE_CURVE ( 'NONE', #11675, #11700, #2763, .T. ) ;
#4633 = DIRECTION ( 'NONE',  ( 0.9928203230275511881, 0.1196152422706609764, 1.201851678989727817E-16 ) ) ;
#4634 = FACE_BOUND ( 'NONE', #13647, .T. ) ;
#4635 = AXIS2_PLACEMENT_3D ( 'NONE', #140, #8761, #14291 ) ;
#4636 = CARTESIAN_POINT ( 'NONE',  ( 27.12922144900085186, -2.887401855662130146, -4.705209693361160461 ) ) ;
#4637 = ORIENTED_EDGE ( 'NONE', *, *, #2514, .F. ) ;
#4638 = CARTESIAN_POINT ( 'NONE',  ( 26.82912971812489644, -6.258282166232842947, -8.283357778048664244 ) ) ;
#4639 = EDGE_CURVE ( 'NONE', #9144, #579, #128, .T. ) ;
#4640 = CARTESIAN_POINT ( 'NONE',  ( 26.34117031759772942, -2.982346454214467535, -4.705209693361161349 ) ) ;
#4641 = EDGE_LOOP ( 'NONE', ( #15860, #4130, #7079, #3748 ) ) ;
#4642 = DIRECTION ( 'NONE',  ( -1.000000000000000000, -0.000000000000000000, -0.000000000000000000 ) ) ;
#4643 = CARTESIAN_POINT ( 'NONE',  ( 33.76397967447234549, -5.422769698972272678, -8.283357778048664244 ) ) ;
#4644 = DIRECTION ( 'NONE',  ( -1.000000000000000000, 0.000000000000000000, -0.000000000000000000 ) ) ;
#4645 = ORIENTED_EDGE ( 'NONE', *, *, #13736, .F. ) ;
#4646 = CARTESIAN_POINT ( 'NONE',  ( 30.40162818048570514, -5.827866652795590241, -3.283357778048667797 ) ) ;
#4647 = LINE ( 'NONE', #13084, #7743 ) ;
#4648 = CARTESIAN_POINT ( 'NONE',  ( 32.75517961154501023, -5.344437665069116328, 3.627061608673662896 ) ) ;
#4649 = STYLED_ITEM ( 'NONE', ( #16761 ), #755 ) ;
#4650 = ORIENTED_EDGE ( 'NONE', *, *, #2857, .T. ) ;
#4651 = CARTESIAN_POINT ( 'NONE',  ( -4.000000000000000000, 2.309401076758501592, -3.133295621305381307 ) ) ;
#4652 = CARTESIAN_POINT ( 'NONE',  ( -21.03357387009699409, -22.15422581635157684, 15.32066355758547083 ) ) ;
#4653 = DIRECTION ( 'NONE',  ( -1.000000000000000000, -1.065814103640150279E-14, 0.000000000000000000 ) ) ;
#4654 = ORIENTED_EDGE ( 'NONE', *, *, #752, .T. ) ;
#4655 = CARTESIAN_POINT ( 'NONE',  ( 1.500000000000000000, -11.00000000000000000, -3.000000000000000000 ) ) ;
#4656 = ORIENTED_EDGE ( 'NONE', *, *, #3902, .T. ) ;
#4657 = CARTESIAN_POINT ( 'NONE',  ( 0.000000000000000000, 0.000000000000000000, -1.901951201008075243 ) ) ;
#4658 = CARTESIAN_POINT ( 'NONE',  ( 26.82229025357024454, -7.323371595517525812, -5.113484796970862334 ) ) ;
#4659 = ORIENTED_EDGE ( 'NONE', *, *, #2382, .T. ) ;
#4660 = CARTESIAN_POINT ( 'NONE',  ( 26.73899421642883567, -2.634607751922174224, -4.533357778048659803 ) ) ;
#4661 = CARTESIAN_POINT ( 'NONE',  ( 33.27992013083530054, -6.934902899450660740, -5.783357778048669573 ) ) ;
#4662 = DIRECTION ( 'NONE',  ( -0.000000000000000000, -0.000000000000000000, 1.000000000000000000 ) ) ;
#4663 = APPLICATION_PROTOCOL_DEFINITION ( 'draft international standard', 'automotive_design', 1998, #15714 ) ;
#4664 = DIRECTION ( 'NONE',  ( -0.000000000000000000, -0.000000000000000000, -1.000000000000000000 ) ) ;
#4665 = CARTESIAN_POINT ( 'NONE',  ( 33.33308377457396432, -5.274811626130743392, -3.627061608673668225 ) ) ;
#4666 = CIRCLE ( 'NONE', #14810, 6.000000000000000888 ) ;
#4667 = EDGE_CURVE ( 'NONE', #7301, #9127, #15277, .T. ) ;
#4668 = FACE_OUTER_BOUND ( 'NONE', #87, .T. ) ;
#4669 = CARTESIAN_POINT ( 'NONE',  ( 29.42969845347704450, -5.944964990802679594, 3.283357778048663356 ) ) ;
#4670 = CARTESIAN_POINT ( 'NONE',  ( 30.18087924896149588, -5.654590020340094725, 7.939653947423658487 ) ) ;
#4671 = ORIENTED_EDGE ( 'NONE', *, *, #16092, .T. ) ;
#4672 = CARTESIAN_POINT ( 'NONE',  ( 26.27285561281998483, -7.029948842322404801, 6.856036165127777693 ) ) ;
#4673 = EDGE_LOOP ( 'NONE', ( #241, #2605, #11554 ) ) ;
#4674 = CARTESIAN_POINT ( 'NONE',  ( 32.81641299864316608, -4.083119185552795294, 3.627061608673664228 ) ) ;
#4675 = CARTESIAN_POINT ( 'NONE',  ( 0.000000000000000000, 0.000000000000000000, 0.000000000000000000 ) ) ;
#4676 = DIRECTION ( 'NONE',  ( 0.9928203230275512992, 0.1196152422706610180, 4.006172263299093133E-17 ) ) ;
#4677 = EDGE_LOOP ( 'NONE', ( #14561, #4388, #713, #2268 ) ) ;
#4678 = AXIS2_PLACEMENT_3D ( 'NONE', #2662, #1218, #9362 ) ;
#4679 = AXIS2_PLACEMENT_3D ( 'NONE', #99, #2549, #8172 ) ;
#4680 = CARTESIAN_POINT ( 'NONE',  ( -4.000000000000000000, -0.8232522521399842086, -3.130632262998158666 ) ) ;
#4681 = CARTESIAN_POINT ( 'NONE',  ( 1.243649364574536075E-15, 4.862606272033089816, -3.445885042887437244 ) ) ;
#4682 = CARTESIAN_POINT ( 'NONE',  ( 32.55256711014040150, -6.632986398338614364, -6.453230759126470595 ) ) ;
#4683 =( BOUNDED_CURVE ( )  B_SPLINE_CURVE ( 3, ( #15233, #5522, #17733, #11124 ),
 .UNSPECIFIED., .F., .T. ) 
 B_SPLINE_CURVE_WITH_KNOTS ( ( 4, 4 ),
 ( 1.825438360997748255, 1.919862177193756514 ),
 .UNSPECIFIED. ) 
 CURVE ( )  GEOMETRIC_REPRESENTATION_ITEM ( )  RATIONAL_B_SPLINE_CURVE ( ( 1.000000000000000000, 0.9992571499088201969, 0.9992571499088201969, 1.000000000000000000 ) ) 
 REPRESENTATION_ITEM ( '' )  );
#4684 = CARTESIAN_POINT ( 'NONE',  ( 28.16881664323205570, -6.096876348486420127, -8.283357778048662468 ) ) ;
#4685 = DIRECTION ( 'NONE',  ( 1.000000000000000000, 0.000000000000000000, 0.000000000000000000 ) ) ;
#4686 = CIRCLE ( 'NONE', #633, 3.999999999999998224 ) ;
#4687 = CARTESIAN_POINT ( 'NONE',  ( 41.60261161686052134, -0.5064767720214736757, -5.783357778048662468 ) ) ;
#4688 = APPLICATION_PROTOCOL_DEFINITION ( 'draft international standard', 'automotive_design', 1998, #17711 ) ;
#4689 = CARTESIAN_POINT ( 'NONE',  ( 28.86293393808771057, -2.678523738846987357, -4.705209693361161349 ) ) ;
#4690 = ADVANCED_FACE ( 'NONE', ( #3578 ), #17647, .F. ) ;
#4691 = CARTESIAN_POINT ( 'NONE',  ( 25.77386970449396841, -2.888308184441632953, -6.623114134516397300 ) ) ;
#4692 = CARTESIAN_POINT ( 'NONE',  ( 30.66050125466253107, -2.889050389913576655, 8.283357778048664244 ) ) ;
#4693 = VERTEX_POINT ( 'NONE', #6100 ) ;
#4694 = EDGE_LOOP ( 'NONE', ( #4150, #4234, #13797 ) ) ;
#4695 = EDGE_LOOP ( 'NONE', ( #4214, #9797, #8476, #3359 ) ) ;
#4696 = AXIS2_PLACEMENT_3D ( 'NONE', #10834, #2700, #3884 ) ;
#4697 = CARTESIAN_POINT ( 'NONE',  ( 32.95662993491456660, -6.574107945067995118, 5.783357778048657138 ) ) ;
#4698 =( NAMED_UNIT ( * ) PLANE_ANGLE_UNIT ( ) SI_UNIT ( $, .RADIAN. ) );
#4699 = CARTESIAN_POINT ( 'NONE',  ( -15.38839387855823126, 12.77214111725050216, -16.22946975555079163 ) ) ;
#4700 = TOROIDAL_SURFACE ( 'NONE', #9899, 2.700000000000000622, 0.2000000000000000111 ) ;
#4701 = DIRECTION ( 'NONE',  ( -1.000000000000000000, 0.000000000000000000, 0.000000000000000000 ) ) ;
#4702 = CARTESIAN_POINT ( 'NONE',  ( 32.67619606237177265, -1.592130426037603907, -5.783357778048658027 ) ) ;
#4703 = DIRECTION ( 'NONE',  ( -0.000000000000000000, -0.000000000000000000, 1.000000000000000000 ) ) ;
#4704 = CARTESIAN_POINT ( 'NONE',  ( 27.24868051476284236, -2.235842002054281075, -6.453230759126464378 ) ) ;
#4705 = AXIS2_PLACEMENT_3D ( 'NONE', #7949, #786, #16211 ) ;
#4706 = FACE_OUTER_BOUND ( 'NONE', #879, .T. ) ;
#4707 = CARTESIAN_POINT ( 'NONE',  ( 36.07773319708005744, -23.32620662758124297, -11.14818368178938357 ) ) ;
#4708 =( BOUNDED_CURVE ( )  B_SPLINE_CURVE ( 2, ( #5386, #13398, #10902, #4139, #16470, #14763, #2348, #7867, #980 ),
 .UNSPECIFIED., .F., .T. ) 
 B_SPLINE_CURVE_WITH_KNOTS ( ( 3, 2, 2, 2, 3 ),
 ( 0.4038461538461538547, 0.4102564102564102422, 0.4230769230769230727, 0.4358974358974359031, 0.4423076923076923461 ),
 .UNSPECIFIED. ) 
 CURVE ( )  GEOMETRIC_REPRESENTATION_ITEM ( )  RATIONAL_B_SPLINE_CURVE ( ( 0.9330127018922194093, 0.9330127018922196314, 1.000000000000000000, 0.8660254037844387076, 1.000000000000000000, 0.8660254037844387076, 1.000000000000000000, 0.9330127018922190762, 0.9330127018922194093 ) ) 
 REPRESENTATION_ITEM ( '' )  );
#4709 = ORIENTED_EDGE ( 'NONE', *, *, #14626, .T. ) ;
#4710 = ORIENTED_EDGE ( 'NONE', *, *, #1345, .F. ) ;
#4711 = CARTESIAN_POINT ( 'NONE',  ( 26.84461768998868436, -2.294720455324902542, -5.783357778048658027 ) ) ;
#4712 = CARTESIAN_POINT ( 'NONE',  ( 25.74999999999999645, -16.21813761408365195, 0.000000000000000000 ) ) ;
#4713 = DIRECTION ( 'NONE',  ( -0.000000000000000000, -0.000000000000000000, 1.000000000000000000 ) ) ;
#4714 = ADVANCED_FACE ( 'NONE', ( #17003 ), #7655, .T. ) ;
#4715 = CIRCLE ( 'NONE', #7046, 2.749999999999988454 ) ;
#4716 = CARTESIAN_POINT ( 'NONE',  ( 28.75424055680402802, -6.753251120556833520, 4.533357778048659803 ) ) ;
#4717 =( BOUNDED_CURVE ( )  B_SPLINE_CURVE ( 2, ( #13140, #10748, #16058, #6334, #7700, #13319, #13226, #14607, #2093 ),
 .UNSPECIFIED., .F., .T. ) 
 B_SPLINE_CURVE_WITH_KNOTS ( ( 3, 2, 2, 2, 3 ),
 ( 0.4807692307692307820, 0.4871794871794871695, 0.5000000000000000000, 0.5128205128205127750, 0.5192307692307692735 ),
 .UNSPECIFIED. ) 
 CURVE ( )  GEOMETRIC_REPRESENTATION_ITEM ( )  RATIONAL_B_SPLINE_CURVE ( ( 0.9330127018922194093, 0.9330127018922196314, 1.000000000000000000, 0.8660254037844387076, 1.000000000000000000, 0.8660254037844387076, 1.000000000000000000, 0.9330127018922187432, 0.9330127018922192983 ) ) 
 REPRESENTATION_ITEM ( '' )  );
#4718 = ORIENTED_EDGE ( 'NONE', *, *, #17640, .T. ) ;
#4719 = CARTESIAN_POINT ( 'NONE',  ( -2.500000000000000888, 0.000000000000000000, -4.674599999999997202 ) ) ;
#4720 = EDGE_CURVE ( 'NONE', #714, #6066, #17381, .T. ) ;
#4721 = CARTESIAN_POINT ( 'NONE',  ( 32.77709966008947617, -5.968767264923789284, -6.861505862736166250 ) ) ;
#4722 = ORIENTED_EDGE ( 'NONE', *, *, #2584, .T. ) ;
#4723 = PLANE ( 'NONE',  #4366 ) ;
#4724 = CIRCLE ( 'NONE', #7916, 2.041999999999999815 ) ;
#4725 = CARTESIAN_POINT ( 'NONE',  ( 26.18940839444933033, -6.337336286969802224, -7.823481096485427777 ) ) ;
#4726 = CARTESIAN_POINT ( 'NONE',  ( -25.11802603177690330, -19.03270077640482683, 10.53798182577225084 ) ) ;
#4727 = CARTESIAN_POINT ( 'NONE',  ( 28.41655006632555569, -6.494127376913395366, -4.705209693361169343 ) ) ;
#4728 = LINE ( 'NONE', #12984, #8364 ) ;
#4729 = CARTESIAN_POINT ( 'NONE',  ( 28.35948656569675919, -3.366149737736551906, -3.627061608673662896 ) ) ;
#4730 = CARTESIAN_POINT ( 'NONE',  ( 27.81599742762458050, -2.504850134108091098, -7.033357778048658027 ) ) ;
#4731 = CARTESIAN_POINT ( 'NONE',  ( 20.00000000000000355, 7.999999999999996447, 0.000000000000000000 ) ) ;
#4732 = PLANE ( 'NONE',  #1386 ) ;
#4733 = CARTESIAN_POINT ( 'NONE',  ( 29.27960797773944179, -6.689954721521948144, -4.533357778048668685 ) ) ;
#4734 = ADVANCED_FACE ( 'NONE', ( #14367 ), #489, .T. ) ;
#4735 = DIRECTION ( 'NONE',  ( -0.000000000000000000, -0.000000000000000000, -1.000000000000000000 ) ) ;
#4736 = CARTESIAN_POINT ( 'NONE',  ( 33.38562051666750818, -5.268481986227246061, 3.627061608673662896 ) ) ;
#4737 = EDGE_CURVE ( 'NONE', #7494, #9058, #13179, .T. ) ;
#4738 = ADVANCED_FACE ( 'NONE', ( #17098 ), #2038, .T. ) ;
#4739 = ORIENTED_EDGE ( 'NONE', *, *, #15462, .F. ) ;
#4740 = FACE_OUTER_BOUND ( 'NONE', #10670, .T. ) ;
#4741 = CARTESIAN_POINT ( 'NONE',  ( 0.000000000000000000, 2.357898499370432166, -2.385244779468109755E-15 ) ) ;
#4742 = FACE_OUTER_BOUND ( 'NONE', #14919, .T. ) ;
#4743 = ORIENTED_EDGE ( 'NONE', *, *, #9181, .T. ) ;
#4744 = CARTESIAN_POINT ( 'NONE',  ( 33.66004903264008874, -1.463398710186760487, -5.783357778048663356 ) ) ;
#4745 = CARTESIAN_POINT ( 'NONE',  ( 25.76974524478944062, -2.854074692636065169, -5.141149657938114181 ) ) ;
#4746 = CARTESIAN_POINT ( 'NONE',  ( 26.31065902414478330, -7.328232685206446106, -6.312034385895062272 ) ) ;
#4747 = LINE ( 'NONE', #10272, #5571 ) ;
#4748 = CARTESIAN_POINT ( 'NONE',  ( 29.49727470010032704, -7.390636972501882340, -5.783357778048669573 ) ) ;
#4749 = CARTESIAN_POINT ( 'NONE',  ( 0.000000000000000000, 0.000000000000000000, -2.000000000000000000 ) ) ;
#4750 = CARTESIAN_POINT ( 'NONE',  ( -6.000000000000000888, 0.000000000000000000, -3.000000000000000000 ) ) ;
#4751 = AXIS2_PLACEMENT_3D ( 'NONE', #8662, #15369, #7043 ) ;
#4752 = CARTESIAN_POINT ( 'NONE',  ( 28.30694982360322953, -3.372479377640031473, -7.939653947423660263 ) ) ;
#4753 = EDGE_CURVE ( 'NONE', #6357, #4375, #2181, .T. ) ;
#4754 = CARTESIAN_POINT ( 'NONE',  ( 27.17934203385504333, -30.00000000000000355, 0.000000000000000000 ) ) ;
#4755 = LINE ( 'NONE', #1789, #13843 ) ;
#4756 = CARTESIAN_POINT ( 'NONE',  ( 28.08810621022444920, -4.652786776866828511, 7.939653947423662039 ) ) ;
#4757 = VERTEX_POINT ( 'NONE', #14458 ) ;
#4758 = CARTESIAN_POINT ( 'NONE',  ( 27.08121146544255353, -6.028038774645947839, -7.939653947423664704 ) ) ;
#4759 = ORIENTED_EDGE ( 'NONE', *, *, #13089, .T. ) ;
#4760 = CARTESIAN_POINT ( 'NONE',  ( 33.30663696749426350, -1.516174747195733863, 5.783357778048668685 ) ) ;
#4761 = CARTESIAN_POINT ( 'NONE',  ( -22.62696978904229184, -9.966234395617776798, 15.00355996101822242 ) ) ;
#4762 = LINE ( 'NONE', #17223, #4136 ) ;
#4763 = ORIENTED_EDGE ( 'NONE', *, *, #10602, .T. ) ;
#4764 = CARTESIAN_POINT ( 'NONE',  ( 4.000000000000000000, -0.3979232138631215721, -1.387439967602543955E-15 ) ) ;
#4765 = CARTESIAN_POINT ( 'NONE',  ( 1.500000000000000222, 9.380831519646861238, -2.000000000000000000 ) ) ;
#4766 = ADVANCED_FACE ( 'NONE', ( #4740 ), #4821, .T. ) ;
#4767 = EDGE_LOOP ( 'NONE', ( #16983, #239, #9851 ) ) ;
#4768 = CARTESIAN_POINT ( 'NONE',  ( 3.510273485745309507, 2.827716139362654424, -3.310536846335887962 ) ) ;
#4769 = CARTESIAN_POINT ( 'NONE',  ( 33.33308377457396432, -5.274811626130743392, -3.627061608673668225 ) ) ;
#4770 = ORIENTED_EDGE ( 'NONE', *, *, #12443, .T. ) ;
#4771 = CARTESIAN_POINT ( 'NONE',  ( 26.78782184427022983, -4.809445364374452581, -8.283357778048662468 ) ) ;
#4772 = CARTESIAN_POINT ( 'NONE',  ( 31.34233605952372415, -6.778795339760710803, 5.783357778048664244 ) ) ;
#4773 = DIRECTION ( 'NONE',  ( 0.000000000000000000, 0.000000000000000000, -1.000000000000000000 ) ) ;
#4774 = SURFACE_STYLE_FILL_AREA ( #17235 ) ;
#4775 = CARTESIAN_POINT ( 'NONE',  ( 29.39282811755836633, -5.749534618892433002, -3.627061608673667781 ) ) ;
#4776 = ORIENTED_EDGE ( 'NONE', *, *, #13426, .F. ) ;
#4777 = CARTESIAN_POINT ( 'NONE',  ( 3.538288549924106796, -15.34800872113743431, 16.99955934415557479 ) ) ;
#4778 = CARTESIAN_POINT ( 'NONE',  ( 32.93832978346670615, -1.887710243310447567, 4.533357778048667797 ) ) ;
#4779 = ORIENTED_EDGE ( 'NONE', *, *, #2478, .F. ) ;
#4780 = VERTEX_POINT ( 'NONE', #10177 ) ;
#4781 = ORIENTED_EDGE ( 'NONE', *, *, #9449, .T. ) ;
#4782 =( GEOMETRIC_REPRESENTATION_CONTEXT ( 3 ) GLOBAL_UNCERTAINTY_ASSIGNED_CONTEXT ( ( #8291 ) ) GLOBAL_UNIT_ASSIGNED_CONTEXT ( ( #9216, #11751, #10645 ) ) REPRESENTATION_CONTEXT ( 'NONE', 'WORKASPACE' ) );
#4783 = DIRECTION ( 'NONE',  ( 0.1196152422706621143, -0.9928203230275509661, 0.000000000000000000 ) ) ;
#4784 = CARTESIAN_POINT ( 'NONE',  ( -8.968477750016525363, -19.11972035685536042, -16.82776078363834671 ) ) ;
#4785 =( BOUNDED_CURVE ( )  B_SPLINE_CURVE ( 2, ( #637, #7706, #10412 ),
 .UNSPECIFIED., .F., .T. ) 
 B_SPLINE_CURVE_WITH_KNOTS ( ( 3, 3 ),
 ( 0.000000000000000000, 1.000000000000000000 ),
 .UNSPECIFIED. ) 
 CURVE ( )  GEOMETRIC_REPRESENTATION_ITEM ( )  RATIONAL_B_SPLINE_CURVE ( ( 0.9436786787937823107, 0.9410169847269389543, 0.9390195162974519505 ) ) 
 REPRESENTATION_ITEM ( '' )  );
#4786 = DIRECTION ( 'NONE',  ( -1.000000000000000000, 0.000000000000000000, 0.000000000000000000 ) ) ;
#4787 = FACE_OUTER_BOUND ( 'NONE', #5956, .T. ) ;
#4788 = EDGE_CURVE ( 'NONE', #12819, #43, #8619, .T. ) ;
#4789 = CARTESIAN_POINT ( 'NONE',  ( -16.91320375285265953, -17.65223671300078223, -16.01217750721622579 ) ) ;
#4790 = CARTESIAN_POINT ( 'NONE',  ( 31.54230778485832332, -2.355712103769039611, -4.705209693361160461 ) ) ;
#4791 = FACE_OUTER_BOUND ( 'NONE', #12767, .T. ) ;
#4792 = DIRECTION ( 'NONE',  ( 0.000000000000000000, 0.000000000000000000, 1.000000000000000000 ) ) ;
#4793 = CARTESIAN_POINT ( 'NONE',  ( 26.73899421642883567, -2.634607751922174224, -4.533357778048659803 ) ) ;
#4794 = CARTESIAN_POINT ( 'NONE',  ( 25.89088658894545603, -2.009881179784104965, -5.783357778048658027 ) ) ;
#4795 = ORIENTED_EDGE ( 'NONE', *, *, #12262, .F. ) ;
#4796 = CARTESIAN_POINT ( 'NONE',  ( 33.30663696749426350, -1.516174747195733863, -5.783357778048658027 ) ) ;
#4797 = FACE_BOUND ( 'NONE', #8132, .T. ) ;
#4798 = VERTEX_POINT ( 'NONE', #2136 ) ;
#4799 = LINE ( 'NONE', #6448, #14434 ) ;
#4800 = CARTESIAN_POINT ( 'NONE',  ( 26.66018910156667232, -2.644102211984857842, 7.033357778048666020 ) ) ;
#4801 = ORIENTED_EDGE ( 'NONE', *, *, #13442, .F. ) ;
#4802 = CARTESIAN_POINT ( 'NONE',  ( 0.000000000000000000, -2.357898499370431722, 2.818925648462311528E-15 ) ) ;
#4803 = CARTESIAN_POINT ( 'NONE',  ( 32.75517961154501023, -5.344437665069116328, -7.939653947423662927 ) ) ;
#4804 = VERTEX_POINT ( 'NONE', #10264 ) ;
#4805 =( BOUNDED_CURVE ( )  B_SPLINE_CURVE ( 3, ( #94, #11118, #4262, #9761 ),
 .UNSPECIFIED., .F., .T. ) 
 B_SPLINE_CURVE_WITH_KNOTS ( ( 4, 4 ),
 ( 1.230954889131919305, 1.393542617697868691 ),
 .UNSPECIFIED. ) 
 CURVE ( )  GEOMETRIC_REPRESENTATION_ITEM ( )  RATIONAL_B_SPLINE_CURVE ( ( 1.000000000000000000, 0.9977983154653933262, 0.9977983154653933262, 1.000000000000000000 ) ) 
 REPRESENTATION_ITEM ( '' )  );
#4806 = EDGE_CURVE ( 'NONE', #13578, #13615, #10338, .T. ) ;
#4807 = CARTESIAN_POINT ( 'NONE',  ( -34.91377932259078420, -11.86950488720510322, 11.57182824616228878 ) ) ;
#4808 = CARTESIAN_POINT ( 'NONE',  ( 2.500000000000000000, -1.768423874527823125, 1.021000000000002128 ) ) ;
#4809 = VERTEX_POINT ( 'NONE', #580 ) ;
#4810 = CARTESIAN_POINT ( 'NONE',  ( 30.01512236704901682, -6.601339762873093875, -7.033357778048666908 ) ) ;
#4811 = APPLICATION_CONTEXT ( 'automotive_design' ) ;
#4812 = CARTESIAN_POINT ( 'NONE',  ( 26.66961417369883591, -4.823687054261037055, -3.627061608673664672 ) ) ;
#4813 = DIRECTION ( 'NONE',  ( -0.9928203230275511881, -0.1196152422706610041, -4.006172263299093133E-17 ) ) ;
#4814 = CARTESIAN_POINT ( 'NONE',  ( -4.281152949374566141, -4.203775615332181026, -3.000000000000000888 ) ) ;
#4815 = CARTESIAN_POINT ( 'NONE',  ( 27.19802975513453092, -2.241944418315925613, 5.783357778048667797 ) ) ;
#4816 = CARTESIAN_POINT ( 'NONE',  ( 27.52714686987067694, -7.627998469090175426, -5.783357778048669573 ) ) ;
#4817 = CARTESIAN_POINT ( 'NONE',  ( 31.75254397038802878, -4.211294393702175398, -8.283357778048662468 ) ) ;
#4818 = CARTESIAN_POINT ( 'NONE',  ( 31.08270050955629671, -4.291997302367946077, 7.939653947423662039 ) ) ;
#4819 = PRODUCT_DEFINITION_FORMATION_WITH_SPECIFIED_SOURCE ( 'ANY', '', #2317, .NOT_KNOWN. ) ;
#4820 = VERTEX_POINT ( 'NONE', #4916 ) ;
#4821 = CYLINDRICAL_SURFACE ( 'NONE', #5703, 2.500000000000001776 ) ;
#4822 = CARTESIAN_POINT ( 'NONE',  ( 33.23365877489121090, -6.550928303235100891, 5.783357778048664244 ) ) ;
#4823 = CARTESIAN_POINT ( 'NONE',  ( 27.29063000668916672, -2.568146533142987575, 7.033357778048666020 ) ) ;
#4824 = ORIENTED_EDGE ( 'NONE', *, *, #194, .T. ) ;
#4825 = CARTESIAN_POINT ( 'NONE',  ( 26.21953647431484313, -6.587393835875770876, 3.921931135572711113 ) ) ;
#4826 = CYLINDRICAL_SURFACE ( 'NONE', #648, 4.000000000000000000 ) ;
#4827 = FACE_OUTER_BOUND ( 'NONE', #4433, .T. ) ;
#4828 = EDGE_CURVE ( 'NONE', #1377, #16314, #10443, .T. ) ;
#4829 = CONICAL_SURFACE ( 'NONE', #6289, 2.500000000000000888, 0.9599310885968781459 ) ;
#4830 = CARTESIAN_POINT ( 'NONE',  ( 32.17274868998081416, -2.279756424927169345, -4.705209693361160461 ) ) ;
#4831 = CARTESIAN_POINT ( 'NONE',  ( 33.01342578063301403, -4.059383036018435753, 3.283357778048664244 ) ) ;
#4832 = VERTEX_POINT ( 'NONE', #409 ) ;
#4833 = CARTESIAN_POINT ( 'NONE',  ( 30.69058026372202974, -5.793053633118939061, -8.283357778048662468 ) ) ;
#4834 = CARTESIAN_POINT ( 'NONE',  ( -3.000000000000000000, 3.673940397442059868E-16, 1.599999999999998979 ) ) ;
#4835 = EDGE_CURVE ( 'NONE', #12650, #14000, #12203, .T. ) ;
#4836 = ITEM_DEFINED_TRANSFORMATION ( 'NONE', 'NONE', #2211,  #3575 ) ;
#4837 = LINE ( 'NONE', #8843, #12132 ) ;
#4838 = CARTESIAN_POINT ( 'NONE',  ( 29.78250536075762867, -6.329556739422670830, -6.861505862736167138 ) ) ;
#4839 = CYLINDRICAL_SURFACE ( 'NONE', #939, 2.500000000000001776 ) ;
#4840 = CARTESIAN_POINT ( 'NONE',  ( 33.55383270609817714, -5.448088258586239796, 8.283357778048660691 ) ) ;
#4841 = CARTESIAN_POINT ( 'NONE',  ( 26.51200394741821498, -4.842675973971495296, 3.627061608673664228 ) ) ;
#4842 = ORIENTED_EDGE ( 'NONE', *, *, #9184, .T. ) ;
#4843 = AXIS2_PLACEMENT_3D ( 'NONE', #3842, #17572, #7920 ) ;
#4844 = ORIENTED_EDGE ( 'NONE', *, *, #6121, .F. ) ;
#4845 = CARTESIAN_POINT ( 'NONE',  ( 26.00079723459025871, -4.771832887959356562, 7.973898148876339853 ) ) ;
#4846 = ORIENTED_EDGE ( 'NONE', *, *, #3681, .F. ) ;
#4847 = CARTESIAN_POINT ( 'NONE',  ( 26.24062359194589078, -6.129313013101781671, 7.939653947423658487 ) ) ;
#4848 = CARTESIAN_POINT ( 'NONE',  ( -22.21636613273916794, -10.00424398458219066, 15.08813622000165466 ) ) ;
#4849 = ORIENTED_EDGE ( 'NONE', *, *, #17295, .F. ) ;
#4850 = DIRECTION ( 'NONE',  ( 1.000000000000000000, 0.000000000000000000, 0.000000000000000000 ) ) ;
#4851 = ORIENTED_EDGE ( 'NONE', *, *, #4267, .F. ) ;
#4852 = FACE_OUTER_BOUND ( 'NONE', #10156, .T. ) ;
#4853 = ADVANCED_FACE ( 'NONE', ( #8329 ), #6374, .F. ) ;
#4854 = DIRECTION ( 'NONE',  ( -0.9928203230275510771, 0.1196152422706621282, 0.000000000000000000 ) ) ;
#4855 = CARTESIAN_POINT ( 'NONE',  ( 36.27615609941022257, -23.17738945083361557, 11.07596365154449636 ) ) ;
#4856 = CARTESIAN_POINT ( 'NONE',  ( 30.67110321781257909, -3.087645581983020637, -7.939653947423660263 ) ) ;
#4857 = CIRCLE ( 'NONE', #9486, 13.00000000000000178 ) ;
#4858 = CARTESIAN_POINT ( 'NONE',  ( 4.203833317240879275, 1.627343821129583867, -3.297273115243890995 ) ) ;
#4859 = LINE ( 'NONE', #1060, #11852 ) ;
#4860 = EDGE_CURVE ( 'NONE', #2226, #8959, #8646, .T. ) ;
#4861 = SURFACE_SIDE_STYLE ('',( #2431 ) ) ;
#4862 = CARTESIAN_POINT ( 'NONE',  ( 26.21417678486618641, -2.370676134166772808, -5.783357778048658027 ) ) ;
#4863 = CARTESIAN_POINT ( 'NONE',  ( -35.41536221060850664, -16.03270077640482683, 0.5379818257722508434 ) ) ;
#4864 = AXIS2_PLACEMENT_3D ( 'NONE', #1182, #10671, #8062 ) ;
#4865 = CARTESIAN_POINT ( 'NONE',  ( 31.88017671309158274, -6.376637546091784792, 7.033357778048657138 ) ) ;
#4866 = EDGE_CURVE ( 'NONE', #7917, #4619, #1992, .T. ) ;
#4867 = ORIENTED_EDGE ( 'NONE', *, *, #12700, .T. ) ;
#4868 = ORIENTED_EDGE ( 'NONE', *, *, #10123, .F. ) ;
#4869 = AXIS2_PLACEMENT_3D ( 'NONE', #14029, #7147, #15291 ) ;
#4870 = ORIENTED_EDGE ( 'NONE', *, *, #10691, .F. ) ;
#4871 = CARTESIAN_POINT ( 'NONE',  ( 26.36761712467744090, -6.740983333149474177, 6.861505862736158257 ) ) ;
#4872 = AXIS2_PLACEMENT_3D ( 'NONE', #17302, #2059, #14475 ) ;
#4873 = CARTESIAN_POINT ( 'NONE',  ( 35.41536221060850664, -16.03270077640482683, 0.5379818257722508434 ) ) ;
#4874 = ORIENTED_EDGE ( 'NONE', *, *, #15623, .T. ) ;
#4875 = CARTESIAN_POINT ( 'NONE',  ( 33.48062616923409252, 0.02583177435456097265, -5.783357778048662468 ) ) ;
#4876 = LINE ( 'NONE', #6431, #9811 ) ;
#4877 = CARTESIAN_POINT ( 'NONE',  ( -26.11936545685874833, -21.64910423302892895, -14.20663795870742696 ) ) ;
#4878 = CARTESIAN_POINT ( 'NONE',  ( 27.77288575766320378, -4.690764616287755651, -7.939653947423662039 ) ) ;
#4879 = CARTESIAN_POINT ( 'NONE',  ( 31.08079519141086067, -2.838413270685653078, -8.283357778048660691 ) ) ;
#4880 = CARTESIAN_POINT ( 'NONE',  ( 27.26436163736424945, -2.571311352887278190, -7.033357778048658027 ) ) ;
#4881 = LINE ( 'NONE', #117, #2152 ) ;
#4882 = DIRECTION ( 'NONE',  ( -0.6951637808321682321, 0.2969442527608448512, 0.6546536707079773088 ) ) ;
#4883 = FACE_OUTER_BOUND ( 'NONE', #8544, .T. ) ;
#4884 = ORIENTED_EDGE ( 'NONE', *, *, #1194, .F. ) ;
#4885 = ORIENTED_EDGE ( 'NONE', *, *, #17671, .T. ) ;
#4886 = CARTESIAN_POINT ( 'NONE',  ( 26.21417678486618641, -2.370676134166772808, -5.783357778048658027 ) ) ;
#4887 = CARTESIAN_POINT ( 'NONE',  ( 31.87075164095941915, -4.197052703815608687, -3.627061608673664672 ) ) ;
#4888 = ORIENTED_EDGE ( 'NONE', *, *, #14108, .T. ) ;
#4889 = DIRECTION ( 'NONE',  ( 0.9928203230275512992, 0.1196152422706610180, 4.006172263299093133E-17 ) ) ;
#4890 = ADVANCED_FACE ( 'NONE', ( #1030 ), #5599, .F. ) ;
#4891 = CARTESIAN_POINT ( 'NONE',  ( -35.41536221060850664, -16.03270077640482683, -0.5379818257722508434 ) ) ;
#4892 = CIRCLE ( 'NONE', #2015, 2.100000000000000089 ) ;
#4893 = PRODUCT_DEFINITION_SHAPE ( 'NONE', 'NONE',  #17985 ) ;
#4894 =( BOUNDED_CURVE ( )  B_SPLINE_CURVE ( 2, ( #7813, #4993, #7904, #828, #10427, #923, #4902, #17271, #7549 ),
 .UNSPECIFIED., .F., .T. ) 
 B_SPLINE_CURVE_WITH_KNOTS ( ( 3, 2, 2, 2, 3 ),
 ( 0.3269230769230769273, 0.3333333333333333148, 0.3461538461538461453, 0.3589743589743589758, 0.3653846153846154188 ),
 .UNSPECIFIED. ) 
 CURVE ( )  GEOMETRIC_REPRESENTATION_ITEM ( )  RATIONAL_B_SPLINE_CURVE ( ( 0.9330127018922194093, 0.9330127018922194093, 1.000000000000000000, 0.8660254037844387076, 1.000000000000000000, 0.8660254037844387076, 1.000000000000000000, 0.9330127018922190762, 0.9330127018922194093 ) ) 
 REPRESENTATION_ITEM ( '' )  );
#4895 = VERTEX_POINT ( 'NONE', #10612 ) ;
#4896 = CARTESIAN_POINT ( 'NONE',  ( 32.36819060393585801, 0.8990368551114588103, 5.783357778048663356 ) ) ;
#4897 = CARTESIAN_POINT ( 'NONE',  ( 33.27602027394517847, -2.146833986953896822, -4.705209693361161349 ) ) ;
#4898 = VERTEX_POINT ( 'NONE', #2222 ) ;
#4899 = CIRCLE ( 'NONE', #9521, 13.00000000000000178 ) ;
#4900 = CARTESIAN_POINT ( 'NONE',  ( 2.500000000000000000, -2.629050547790028551E-15, -2.041999999999999815 ) ) ;
#4901 = EDGE_CURVE ( 'NONE', #9400, #4376, #14993, .T. ) ;
#4902 = CARTESIAN_POINT ( 'NONE',  ( 31.27600417729400917, -6.449428405189353342, -7.033357778048666908 ) ) ;
#4903 = VERTEX_POINT ( 'NONE', #16685 ) ;
#4904 = B_SPLINE_CURVE_WITH_KNOTS ( 'NONE', 3,
 ( #11646, #3319, #8932, #14474 ),
 .UNSPECIFIED., .F., .F.,
 ( 4, 4 ),
 ( 2.843119637691541009E-07, 0.001422633878257847061 ),
 .UNSPECIFIED. ) ;
#4905 = CARTESIAN_POINT ( 'NONE',  ( 31.12210306526553083, -4.287250072544045665, -8.283357778048662468 ) ) ;
#4906 = CIRCLE ( 'NONE', #1740, 5.500000000000000888 ) ;
#4907 = CARTESIAN_POINT ( 'NONE',  ( 27.61527553138257574, -4.709753535998224550, -7.939653947423662039 ) ) ;
#4908 = DIRECTION ( 'NONE',  ( 0.000000000000000000, 0.000000000000000000, 1.000000000000000000 ) ) ;
#4909 = CARTESIAN_POINT ( 'NONE',  ( 33.47428445112562656, -1.485779673698264913, -6.453230759126466154 ) ) ;
#4910 = CARTESIAN_POINT ( 'NONE',  ( 14.05146698326616672, 13.69412420653798357, -16.38624388364804219 ) ) ;
#4911 = CARTESIAN_POINT ( 'NONE',  ( 28.05993251931039012, -3.202367565343739564, -3.283357778048662023 ) ) ;
#4912 = ADVANCED_FACE ( 'NONE', ( #10533 ), #14728, .F. ) ;
#4913 = CARTESIAN_POINT ( 'NONE',  ( 31.71314141467879111, -4.216041623526076698, -3.627061608673664672 ) ) ;
#4914 = EDGE_CURVE ( 'NONE', #17268, #5050, #2552, .T. ) ;
#4915 = ORIENTED_EDGE ( 'NONE', *, *, #5443, .F. ) ;
#4916 = CARTESIAN_POINT ( 'NONE',  ( 38.62415064777786000, -0.8653224988334575762, -5.783357778048662468 ) ) ;
#4917 = CARTESIAN_POINT ( 'NONE',  ( -20.00000000000000355, 7.999999999999996447, -6.000000000000000000 ) ) ;
#4918 = CARTESIAN_POINT ( 'NONE',  ( 0.000000000000000000, 0.000000000000000000, -2.000000000000000000 ) ) ;
#4919 = ORIENTED_EDGE ( 'NONE', *, *, #15167, .T. ) ;
#4920 = DIRECTION ( 'NONE',  ( 0.000000000000000000, -0.000000000000000000, 1.000000000000000000 ) ) ;
#4921 = CLOSED_SHELL ( 'NONE', ( #14723, #11343, #5574, #299, #7162, #12345, #15169, #8943, #5640, #2440, #8741, #4421, #3827, #15310, #1715, #5899, #9694, #9871, #14974, #3996, #17071, #4149, #12517, #7789, #10053, #6574, #16477, #10176, #2580, #11112, #2907, #7430, #16188, #5773, #6399, #7008, #5061, #12655, #3922, #7194, #13967, #5404, #5812, #14815, #17275, #12865, #15795, #6922, #772, #16257, #9813, #7351, #15545, #256, #4220, #14755, #16780, #4958, #15727, #10719, #4182, #16494, #11611, #7671, #6134, #14062, #2279, #14197, #569, #16451, #16677, #12305, #16378, #11528, #13637, #11195, #17590, #14086, #14777, #16409, #9048, #16540, #13841, #850, #7516, #12824, #4912, #16500, #230, #10219, #10986, #9784, #4853, #6605, #6949, #98, #8169, #5788, #5625, #17466, #10433, #173, #12497, #7126, #10625, #10454, #4571, #13728, #1208 ) ) ;
#4922 = CARTESIAN_POINT ( 'NONE',  ( 25.78162057792670225, -2.952641328940847743, -4.882123357130833341 ) ) ;
#4923 = CARTESIAN_POINT ( 'NONE',  ( 31.87075164095941915, -4.197052703815608687, -3.627061608673664672 ) ) ;
#4924 = CARTESIAN_POINT ( 'NONE',  ( 1.746467850512308208E-21, -1.591841644184202181E-21, -6.005572809000082835 ) ) ;
#4925 = CARTESIAN_POINT ( 'NONE',  ( 27.99987602667382802, -2.482696394238434578, -4.533357778048659803 ) ) ;
#4926 = FACE_OUTER_BOUND ( 'NONE', #11004, .T. ) ;
#4927 = DIRECTION ( 'NONE',  ( 0.000000000000000000, 0.000000000000000000, 1.000000000000000000 ) ) ;
#4928 = LINE ( 'NONE', #14905, #3978 ) ;
#4929 = CARTESIAN_POINT ( 'NONE',  ( 31.24031073583692475, -4.273008382657478954, -3.627061608673664672 ) ) ;
#4930 = CARTESIAN_POINT ( 'NONE',  ( 0.000000000000000000, 0.000000000000000000, -4.184454397937119374 ) ) ;
#4931 = CARTESIAN_POINT ( 'NONE',  ( 32.90015225647083952, -1.554951264938056132, 6.453230759126471483 ) ) ;
#4932 = CARTESIAN_POINT ( 'NONE',  ( 33.76397967447234549, -5.422769698972272678, 3.283357778048663800 ) ) ;
#4933 = CIRCLE ( 'NONE', #3205, 6.000000000000000888 ) ;
#4934 = EDGE_CURVE ( 'NONE', #9123, #7189, #5008, .T. ) ;
#4935 = ORIENTED_EDGE ( 'NONE', *, *, #16072, .F. ) ;
#4936 = DIRECTION ( 'NONE',  ( -0.9569661826241284697, -0.2901994578110082545, -1.159531966109436593E-16 ) ) ;
#4937 = ORIENTED_EDGE ( 'NONE', *, *, #8634, .F. ) ;
#4938 = CARTESIAN_POINT ( 'NONE',  ( 31.66930131758986988, -2.967382423816733894, 7.939653947423664704 ) ) ;
#4939 =( LENGTH_UNIT ( ) NAMED_UNIT ( * ) SI_UNIT ( .MILLI., .METRE. ) );
#4940 = FACE_OUTER_BOUND ( 'NONE', #11295, .T. ) ;
#4941 = EDGE_CURVE ( 'NONE', #5360, #16822, #9268, .T. ) ;
#4942 = VERTEX_POINT ( 'NONE', #14640 ) ;
#4943 = VECTOR ( 'NONE', #11781, 1000.000000000000227 ) ;
#4944 = CARTESIAN_POINT ( 'NONE',  ( -2.016448651773435938E-27, -20.49999999999999645, 6.000000000000000000 ) ) ;
#4945 = CARTESIAN_POINT ( 'NONE',  ( 2.500000000000000000, -1.178949249685213863, 2.042000000000001148 ) ) ;
#4946 = DIRECTION ( 'NONE',  ( -1.000000000000000000, 0.000000000000000000, 0.000000000000000000 ) ) ;
#4947 = CARTESIAN_POINT ( 'NONE',  ( -0.6666666666666659635, 4.233901974057258322, -3.000726591567082657 ) ) ;
#4948 = AXIS2_PLACEMENT_3D ( 'NONE', #14139, #5881, #11404 ) ;
#4949 = CARTESIAN_POINT ( 'NONE',  ( 31.88814493096863956, -1.687075024589942851, -5.783357778048658027 ) ) ;
#4950 = CARTESIAN_POINT ( 'NONE',  ( -0.6641139335927965792, 4.471067008845558632, -3.302142222888768686 ) ) ;
#4951 = DIRECTION ( 'NONE',  ( -1.000000000000000000, 0.000000000000000000, 0.000000000000000000 ) ) ;
#4952 = CARTESIAN_POINT ( 'NONE',  ( 28.35948656569675919, -3.366149737736551906, -3.627061608673662896 ) ) ;
#4953 = CARTESIAN_POINT ( 'NONE',  ( 33.12669930479518854, -6.563814807098823145, -5.113484796970860558 ) ) ;
#4954 = LINE ( 'NONE', #11313, #16457 ) ;
#4955 = CARTESIAN_POINT ( 'NONE',  ( -7.374038404636016786, -5.989453865500021124, -2.000000000000000000 ) ) ;
#4956 = VECTOR ( 'NONE', #8576, 1000.000000000000227 ) ;
#4957 = CARTESIAN_POINT ( 'NONE',  ( 31.29094215978502547, -2.813094711071706389, 8.283357778048664244 ) ) ;
#4958 = ADVANCED_FACE ( 'NONE', ( #16272 ), #7828, .T. ) ;
#4959 = ORIENTED_EDGE ( 'NONE', *, *, #11848, .T. ) ;
#4960 = ORIENTED_EDGE ( 'NONE', *, *, #16415, .F. ) ;
#4961 = ORIENTED_EDGE ( 'NONE', *, *, #3357, .T. ) ;
#4962 = VECTOR ( 'NONE', #2640, 1000.000000000000227 ) ;
#4963 = VERTEX_POINT ( 'NONE', #1369 ) ;
#4964 = CARTESIAN_POINT ( 'NONE',  ( 27.45273115869273539, -7.247415916675651992, 6.453230759126468818 ) ) ;
#4965 = CARTESIAN_POINT ( 'NONE',  ( 33.76207435632690590, -3.969185667289998332, 7.939653947423662039 ) ) ;
#4966 = EDGE_CURVE ( 'NONE', #558, #14684, #1359, .T. ) ;
#4967 = ORIENTED_EDGE ( 'NONE', *, *, #12198, .F. ) ;
#4968 = DIRECTION ( 'NONE',  ( 0.000000000000000000, 0.000000000000000000, 1.000000000000000000 ) ) ;
#4969 = CARTESIAN_POINT ( 'NONE',  ( -25.20430036322041545, -22.07000804769847591, -14.42834449896450799 ) ) ;
#4971 = AXIS2_PLACEMENT_3D ( 'NONE', #17742, #14972, #12260 ) ;
#4970 = CARTESIAN_POINT ( 'NONE',  ( 29.04699097144805364, -6.418171698071525100, -4.705209693361169343 ) ) ;
#4972 = CARTESIAN_POINT ( 'NONE',  ( -5.816800114226745675E-16, -4.862606272033100474, -3.445885042887441241 ) ) ;
#4973 = CARTESIAN_POINT ( 'NONE',  ( 8.250000000000014211, 6.495190528383269601, -3.000000000000000000 ) ) ;
#4974 = CARTESIAN_POINT ( 'NONE',  ( -23.00000000000000000, -16.21813761408365195, 13.00000000000000178 ) ) ;
#4975 = CARTESIAN_POINT ( 'NONE',  ( 27.55969062878875064, -7.234529412811931515, 5.783357778048657138 ) ) ;
#4976 = CARTESIAN_POINT ( 'NONE',  ( 17.39700462756752231, -13.41815250082780508, 15.94071721526680108 ) ) ;
#4977 =( NAMED_UNIT ( * ) PLANE_ANGLE_UNIT ( ) SI_UNIT ( $, .RADIAN. ) );
#4978 = ORIENTED_EDGE ( 'NONE', *, *, #12736, .F. ) ;
#4979 = AXIS2_PLACEMENT_3D ( 'NONE', #1121, #13889, #6558 ) ;
#4980 = VECTOR ( 'NONE', #6063, 1000.000000000000000 ) ;
#4981 = CARTESIAN_POINT ( 'NONE',  ( 28.13194630731337753, -5.901445976576171759, -3.627061608673667781 ) ) ;
#4982 = CARTESIAN_POINT ( 'NONE',  ( 30.78487334700428235, -1.819997462563214263, -5.783357778048658915 ) ) ;
#4983 = ORIENTED_EDGE ( 'NONE', *, *, #431, .T. ) ;
#4984 = CARTESIAN_POINT ( 'NONE',  ( -13.00000000000000178, -1.592040838891559293E-15, 12.00000000000000000 ) ) ;
#4985 = CARTESIAN_POINT ( 'NONE',  ( 2.500000000000000000, -2.357898499370431722, 2.818925648462311528E-15 ) ) ;
#4986 = ORIENTED_EDGE ( 'NONE', *, *, #6195, .F. ) ;
#4987 = CARTESIAN_POINT ( 'NONE',  ( 3.999999999999998224, 0.000000000000000000, 0.000000000000000000 ) ) ;
#4988 = CARTESIAN_POINT ( 'NONE',  ( 33.40754056521197413, -5.892811586081919906, -6.861505862736166250 ) ) ;
#4989 = ORIENTED_EDGE ( 'NONE', *, *, #17909, .F. ) ;
#4990 = AXIS2_PLACEMENT_3D ( 'NONE', #8667, #11168, #1788 ) ;
#4991 = AXIS2_PLACEMENT_3D ( 'NONE', #10582, #1001, #14613 ) ;
#4992 = CARTESIAN_POINT ( 'NONE',  ( 29.37220822929407760, -7.016156836349003001, 5.783357778048657138 ) ) ;
#4993 = CARTESIAN_POINT ( 'NONE',  ( 30.95252083063564896, -1.789602389065743981, -6.453230759126464378 ) ) ;
#4994 = ORIENTED_EDGE ( 'NONE', *, *, #11950, .F. ) ;
#4995 = CARTESIAN_POINT ( 'NONE',  ( 29.71979337562451207, -1.938121702948446323, -5.783357778048664244 ) ) ;
#4996 = EDGE_CURVE ( 'NONE', #14967, #17858, #4294, .T. ) ;
#4997 = CARTESIAN_POINT ( 'NONE',  ( 31.17093069310692499, -6.462087684996337345, -4.533357778048668685 ) ) ;
#4998 = CARTESIAN_POINT ( 'NONE',  ( 28.88938074516742205, -6.437160617781993999, -4.705209693361168455 ) ) ;
#4999 = B_SPLINE_CURVE_WITH_KNOTS ( 'NONE', 3,
 ( #12970, #3641, #816, #11780, #6348 ),
 .UNSPECIFIED., .F., .F.,
 ( 4, 1, 4 ),
 ( 4.386880129527780036E-20, 0.002309401076758504055, 0.004618802153517008978 ),
 .UNSPECIFIED. ) ;
#5000 = DIRECTION ( 'NONE',  ( -0.000000000000000000, 1.103561164596346103E-15, 1.000000000000000000 ) ) ;
#5001 = LINE ( 'NONE', #13618, #8686 ) ;
#5002 = CYLINDRICAL_SURFACE ( 'NONE', #7017, 12.50000000000000000 ) ;
#5003 = ORIENTED_EDGE ( 'NONE', *, *, #335, .F. ) ;
#5004 = CARTESIAN_POINT ( 'NONE',  ( 28.48022645605872327, -3.151730446115816875, -8.283357778048658915 ) ) ;
#5005 = VERTEX_POINT ( 'NONE', #4177 ) ;
#5006 = VECTOR ( 'NONE', #14218, 1000.000000000000114 ) ;
#5007 = COLOUR_RGB ( '', 0.40784314, 0.44705882, 0.49803922) ;
#5008 = LINE ( 'NONE', #12412, #10641 ) ;
#5009 = CARTESIAN_POINT ( 'NONE',  ( 29.79859849048667897, -1.928627242885762705, -5.783357778048664244 ) ) ;
#5010 = CARTESIAN_POINT ( 'NONE',  ( -0.6448876103708482965, -4.246476118072356698, -0.2256878752776764752 ) ) ;
#5011 = VECTOR ( 'NONE', #7785, 1000.000000000000000 ) ;
#5012 = EDGE_LOOP ( 'NONE', ( #8756, #11883, #5023, #1923 ) ) ;
#5013 = CARTESIAN_POINT ( 'NONE',  ( 33.68284756902015431, -1.652629194728084450, -1.783357778048662912 ) ) ;
#5014 = CARTESIAN_POINT ( 'NONE',  ( 0.000000000000000000, 0.000000000000000000, 13.31572692736085095 ) ) ;
#5015 = CARTESIAN_POINT ( 'NONE',  ( 33.33308377457396432, -5.274811626130743392, -3.627061608673668225 ) ) ;
#5016 = EDGE_CURVE ( 'NONE', #1330, #16314, #13361, .T. ) ;
#5017 = ORIENTED_EDGE ( 'NONE', *, *, #2636, .T. ) ;
#5018 = CARTESIAN_POINT ( 'NONE',  ( 25.95642634701329499, -4.403549397486640871, -3.686412874245495797 ) ) ;
#5019 = CARTESIAN_POINT ( 'NONE',  ( 29.84999239022537409, -5.894327871574777333, -3.283357778048667797 ) ) ;
#5020 = DIRECTION ( 'NONE',  ( -1.000000000000000000, -0.000000000000000000, -0.000000000000000000 ) ) ;
#5021 = FACE_BOUND ( 'NONE', #13598, .T. ) ;
#5022 = CARTESIAN_POINT ( 'NONE',  ( 0.000000000000000000, 0.000000000000000000, -4.699999999999999289 ) ) ;
#5023 = ORIENTED_EDGE ( 'NONE', *, *, #4293, .T. ) ;
#5024 = CARTESIAN_POINT ( 'NONE',  ( 29.65098506949083301, -2.583579140294649523, -4.705209693361160461 ) ) ;
#5025 = CARTESIAN_POINT ( 'NONE',  ( 34.91377932259078420, -11.86950488720510322, -11.57182824616228878 ) ) ;
#5026 = CARTESIAN_POINT ( 'NONE',  ( -2.016448651773435938E-27, -20.49999999999999645, 13.00000000000000178 ) ) ;
#5027 = CARTESIAN_POINT ( 'NONE',  ( 26.65222088368961195, -7.333664733486695120, 5.783357778048657138 ) ) ;
#5028 = ORIENTED_EDGE ( 'NONE', *, *, #13273, .T. ) ;
#5029 = EDGE_LOOP ( 'NONE', ( #14424, #10557, #1479, #4868 ) ) ;
#5030 = ORIENTED_EDGE ( 'NONE', *, *, #15138, .T. ) ;
#5031 = CARTESIAN_POINT ( 'NONE',  ( 28.91999743871649997, -5.806501378023834370, 7.939653947423658487 ) ) ;
#5032 = DIRECTION ( 'NONE',  ( -0.000000000000000000, -1.000000000000000000, 3.469446951953614189E-16 ) ) ;
#5033 = DIRECTION ( 'NONE',  ( -0.1196152422706611984, 0.9928203230275510771, 0.000000000000000000 ) ) ;
#5034 = VERTEX_POINT ( 'NONE', #942 ) ;
#5035 =( NAMED_UNIT ( * ) PLANE_ANGLE_UNIT ( ) SI_UNIT ( $, .RADIAN. ) );
#5036 = DIRECTION ( 'NONE',  ( -0.000000000000000000, -0.000000000000000000, 1.000000000000000000 ) ) ;
#5037 = EDGE_CURVE ( 'NONE', #7494, #6265, #9676, .T. ) ;
#5038 = PLANE ( 'NONE',  #4705 ) ;
#5039 = LINE ( 'NONE', #7684, #14869 ) ;
#5040 = CARTESIAN_POINT ( 'NONE',  ( 30.62726312072365431, -1.838986382273682718, -5.783357778048658027 ) ) ;
#5041 = CARTESIAN_POINT ( 'NONE',  ( -2.712778981739305095, 3.052578478157828012, -3.130620751972063687 ) ) ;
#5042 = CARTESIAN_POINT ( 'NONE',  ( 33.56434302664245450, -9.029166375164061620, 5.783357778048664244 ) ) ;
#5043 = FILL_AREA_STYLE_COLOUR ( '', #1605 ) ;
#5044 = CARTESIAN_POINT ( 'NONE',  ( 29.62489513447700062, -6.348545659133139729, -6.861505862736166250 ) ) ;
#5045 = DIRECTION ( 'NONE',  ( 0.8660254037844378194, -0.5000000000000014433, 0.000000000000000000 ) ) ;
#5046 = DIRECTION ( 'NONE',  ( -0.000000000000000000, -0.000000000000000000, -1.000000000000000000 ) ) ;
#5047 = CARTESIAN_POINT ( 'NONE',  ( 26.01652455409633902, -4.902371455920936150, 5.783357778048662468 ) ) ;
#5048 = CARTESIAN_POINT ( 'NONE',  ( 28.99436501219896201, -4.543600488427916417, 8.283357778048662468 ) ) ;
#5049 = ORIENTED_EDGE ( 'NONE', *, *, #2082, .T. ) ;
#5050 = VERTEX_POINT ( 'NONE', #7170 ) ;
#5051 = VERTEX_POINT ( 'NONE', #11202 ) ;
#5052 = ORIENTED_EDGE ( 'NONE', *, *, #7774, .F. ) ;
#5054 = B_SPLINE_CURVE_WITH_KNOTS ( 'NONE', 3,
 ( #96, #3167, #3266, #5964, #4442, #9953, #1642, #9763 ),
 .UNSPECIFIED., .F., .F.,
 ( 4, 2, 2, 4 ),
 ( 2.465131517071352357E-07, 0.001183067374689843057, 0.001774477805458910939, 0.002365888236227979037 ),
 .UNSPECIFIED. ) ;
#5053 = LINE ( 'NONE', #11676, #3404 ) ;
#5055 = CARTESIAN_POINT ( 'NONE',  ( 28.30694982360322953, -3.372479377640031473, 3.627061608673666449 ) ) ;
#5056 = VERTEX_POINT ( 'NONE', #8517 ) ;
#5057 = CARTESIAN_POINT ( 'NONE',  ( 50.00000000000000000, -19.03270077640483038, 5.537981825772250843 ) ) ;
#5058 = CARTESIAN_POINT ( 'NONE',  ( 29.17398450417959310, -7.029842018119214941, -5.783357778048669573 ) ) ;
#5059 = LINE ( 'NONE', #16147, #15088 ) ;
#5061 = ADVANCED_FACE ( 'NONE', ( #4608 ), #15500, .F. ) ;
#5060 = CARTESIAN_POINT ( 'NONE',  ( 32.01903832059031174, -7.086814257134402162, -5.783357778048669573 ) ) ;
#5062 = DIRECTION ( 'NONE',  ( 1.224646799147353207E-16, -1.000000000000000000, 0.000000000000000000 ) ) ;
#5063 = CARTESIAN_POINT ( 'NONE',  ( 26.65222088368961195, -7.333664733486695120, -5.783357778048669573 ) ) ;
#5064 = CARTESIAN_POINT ( 'NONE',  ( 21.62432203902686823, -10.11801842300244125, 15.20615207729255403 ) ) ;
#5065 = ORIENTED_EDGE ( 'NONE', *, *, #3938, .F. ) ;
#5066 = CARTESIAN_POINT ( 'NONE',  ( 31.56875459193803124, -6.114348982704044921, -4.705209693361169343 ) ) ;
#5067 = CARTESIAN_POINT ( 'NONE',  ( 32.17274868998081416, -2.279756424927169345, -4.705209693361160461 ) ) ;
#5068 = ORIENTED_EDGE ( 'NONE', *, *, #3627, .T. ) ;
#5069 = EDGE_CURVE ( 'NONE', #7075, #15926, #17188, .T. ) ;
#5070 = DIRECTION ( 'NONE',  ( 1.000000000000000000, 0.000000000000000000, 0.000000000000000000 ) ) ;
#5071 = CARTESIAN_POINT ( 'NONE',  ( 34.23532670761333918, -6.238269840783186027, -9.783357778048662468 ) ) ;
#5072 = ORIENTED_EDGE ( 'NONE', *, *, #16660, .F. ) ;
#5073 = CARTESIAN_POINT ( 'NONE',  ( 3.999999999999999112, 1.563622288139204342, -0.2253451193528351326 ) ) ;
#5074 = CARTESIAN_POINT ( 'NONE',  ( 32.01513846370018967, -2.298745344637636912, -4.705209693361161349 ) ) ;
#5075 = ORIENTED_EDGE ( 'NONE', *, *, #15167, .F. ) ;
#5076 = DIRECTION ( 'NONE',  ( -1.000000000000000000, 0.000000000000000000, 0.000000000000000000 ) ) ;
#5077 = CARTESIAN_POINT ( 'NONE',  ( 25.94629020164262556, -4.319418220471658465, -8.066408332899133171 ) ) ;
#5078 = CARTESIAN_POINT ( 'NONE',  ( -8.632250723006722026, -18.84644399697197770, 16.84735068286508763 ) ) ;
#5079 = ADVANCED_FACE ( 'NONE', ( #1547 ), #14050, .T. ) ;
#5080 = LINE ( 'NONE', #14714, #14554 ) ;
#5081 = CARTESIAN_POINT ( 'NONE',  ( 32.43181250335191379, -6.310176327312596811, -4.533357778048668685 ) ) ;
#5082 = ORIENTED_EDGE ( 'NONE', *, *, #13089, .F. ) ;
#5083 = CARTESIAN_POINT ( 'NONE',  ( 0.6666666666666668517, 4.233901974057260986, -3.000726591567082657 ) ) ;
#5084 = EDGE_CURVE ( 'NONE', #4359, #7377, #12679, .T. ) ;
#5085 = CARTESIAN_POINT ( 'NONE',  ( 25.90934487712387480, 0.1208734971681841297, -15.78335777804866424 ) ) ;
#5086 = CARTESIAN_POINT ( 'NONE',  ( 32.83754810739939956, -9.116730809865838836, 5.783357778048664244 ) ) ;
#5087 = CARTESIAN_POINT ( 'NONE',  ( 0.000000000000000000, 0.000000000000000000, 1.599999999999999423 ) ) ;
#5088 = CARTESIAN_POINT ( 'NONE',  ( 29.98133424373737910, -5.878503772023492502, -8.283357778048662468 ) ) ;
#5089 = CARTESIAN_POINT ( 'NONE',  ( 31.41114436565740320, -6.133337902414513820, -4.705209693361168455 ) ) ;
#5090 = ADVANCED_FACE ( 'NONE', ( #7434 ), #14130, .T. ) ;
#5091 = ORIENTED_EDGE ( 'NONE', *, *, #6986, .F. ) ;
#5092 = CARTESIAN_POINT ( 'NONE',  ( 9.166200962222307069, -3.560057785416429255, -2.333128398347826593 ) ) ;
#5093 = CARTESIAN_POINT ( 'NONE',  ( 33.40745134805642635, -4.011910736534825439, -3.283357778048664688 ) ) ;
#5094 = ORIENTED_EDGE ( 'NONE', *, *, #14365, .F. ) ;
#5095 = CARTESIAN_POINT ( 'NONE',  ( 0.000000000000000000, 0.000000000000000000, 0.000000000000000000 ) ) ;
#5096 = DIRECTION ( 'NONE',  ( -1.224646799147353207E-16, 1.000000000000000000, 0.000000000000000000 ) ) ;
#5097 = LINE ( 'NONE', #8004, #15403 ) ;
#5098 = CARTESIAN_POINT ( 'NONE',  ( 29.78612525785423060, -2.267488637519798012, 4.533357778048667797 ) ) ;
#5099 = EDGE_CURVE ( 'NONE', #5285, #7960, #17353, .T. ) ;
#5100 = CARTESIAN_POINT ( 'NONE',  ( 29.18947247604337392, -3.066280307211263878, -8.283357778048658915 ) ) ;
#5101 = CARTESIAN_POINT ( 'NONE',  ( 26.01652455409633902, -4.902371455920926380, 5.783357778048663356 ) ) ;
#5102 = DIRECTION ( 'NONE',  ( 0.000000000000000000, -1.000000000000000000, 3.469446951953614189E-16 ) ) ;
#5103 = LINE ( 'NONE', #11909, #5688 ) ;
#5104 = ORIENTED_EDGE ( 'NONE', *, *, #12475, .T. ) ;
#5105 = CARTESIAN_POINT ( 'NONE',  ( 29.54591158530375239, -2.596238420101622868, -6.861505862736158257 ) ) ;
#5106 = CARTESIAN_POINT ( 'NONE',  ( 33.40754056521197413, -5.892811586081919906, -6.861505862736166250 ) ) ;
#5107 = CARTESIAN_POINT ( 'NONE',  ( 26.79666222766753592, -21.19920099154242976, -14.03599807436713398 ) ) ;
#5108 = CARTESIAN_POINT ( 'NONE',  ( 26.41562710823574278, -3.600346414165641828, 3.627061608673666893 ) ) ;
#5109 = ADVANCED_FACE ( 'NONE', ( #3163 ), #8602, .F. ) ;
#5110 = VERTEX_POINT ( 'NONE', #11580 ) ;
#5111 = CARTESIAN_POINT ( 'NONE',  ( 30.43486631442457835, -6.877930660435475296, 5.783357778048657138 ) ) ;
#5112 = LINE ( 'NONE', #10554, #14203 ) ;
#5113 = DIRECTION ( 'NONE',  ( 0.000000000000000000, 0.000000000000000000, -1.000000000000000000 ) ) ;
#5114 = EDGE_LOOP ( 'NONE', ( #17335, #908, #6998, #14930 ) ) ;
#5115 = LINE ( 'NONE', #14918, #7074 ) ;
#5116 = CARTESIAN_POINT ( 'NONE',  ( 12.50000000000000000, 1.530808498934191521E-15, -4.000000000000000000 ) ) ;
#5117 = ADVANCED_FACE ( 'NONE', ( #1822 ), #4438, .F. ) ;
#5118 = CARTESIAN_POINT ( 'NONE',  ( 32.32036211097666012, -1.624804527518282748, 5.783357778048663356 ) ) ;
#5119 = DIRECTION ( 'NONE',  ( -0.9928203230275514102, -0.1196152422706598939, 0.000000000000000000 ) ) ;
#5120 = AXIS2_PLACEMENT_3D ( 'NONE', #5718, #11235, #2755 ) ;
#5121 = CARTESIAN_POINT ( 'NONE',  ( 30.75425665345519732, -2.450656702321377001, -4.705209693361161349 ) ) ;
#5122 = LINE ( 'NONE', #17318, #12688 ) ;
#5123 = CARTESIAN_POINT ( 'NONE',  ( -5.781152949374542160, -1.605699403978850803, -3.000000000000000888 ) ) ;
#5124 = APPLICATION_PROTOCOL_DEFINITION ( 'draft international standard', 'automotive_design', 1998, #1118 ) ;
#5125 = CARTESIAN_POINT ( 'NONE',  ( 25.60565592828815440, -3.070961412863312034, 4.705209693361167567 ) ) ;
#5126 = VECTOR ( 'NONE', #124, 1000.000000000000000 ) ;
#5127 = CARTESIAN_POINT ( 'NONE',  ( 33.40745134805642635, -4.011910736534825439, 8.283357778048662468 ) ) ;
#5128 = DIRECTION ( 'NONE',  ( -1.000000000000000000, 0.000000000000000000, 0.000000000000000000 ) ) ;
#5129 = CARTESIAN_POINT ( 'NONE',  ( 47.10521669518294630, -4.378041487036774981, -5.783357778048661579 ) ) ;
#5130 = CARTESIAN_POINT ( 'NONE',  ( 27.50829672905005907, -3.268828784122927100, 8.283357778048664244 ) ) ;
#5131 = EDGE_CURVE ( 'NONE', #17048, #15612, #13262, .T. ) ;
#5132 = ORIENTED_EDGE ( 'NONE', *, *, #12047, .F. ) ;
#5133 = ORIENTED_EDGE ( 'NONE', *, *, #13337, .T. ) ;
#5134 = ORIENTED_EDGE ( 'NONE', *, *, #16914, .T. ) ;
#5135 = CARTESIAN_POINT ( 'NONE',  ( 30.62726312072365431, -1.838986382273682718, 5.783357778048668685 ) ) ;
#5136 = CARTESIAN_POINT ( 'NONE',  ( 30.92509028327567933, -4.310986222078405206, 3.627061608673664228 ) ) ;
#5137 = EDGE_LOOP ( 'NONE', ( #3371, #16922 ) ) ;
#5138 = CARTESIAN_POINT ( 'NONE',  ( 30.61929490284659394, -6.528548903775525325, 7.033357778048657138 ) ) ;
#5139 = VECTOR ( 'NONE', #5641, 1000.000000000000000 ) ;
#5140 = CARTESIAN_POINT ( 'NONE',  ( 30.06013935859953534, -5.869009311960809328, -8.283357778048664244 ) ) ;
#5141 = DIRECTION ( 'NONE',  ( 0.9928203230275512992, 0.1196152422706610180, 4.006172263299093133E-17 ) ) ;
#5142 = CARTESIAN_POINT ( 'NONE',  ( 28.28502977505876359, -2.748149777785362957, -6.861505862736158257 ) ) ;
#5143 = FACE_OUTER_BOUND ( 'NONE', #16053, .T. ) ;
#5144 = DIRECTION ( 'NONE',  ( 1.000000000000000000, 0.000000000000000000, 0.000000000000000000 ) ) ;
#5145 = CARTESIAN_POINT ( 'NONE',  ( 0.000000000000000000, 0.000000000000000000, -2.000000000000000000 ) ) ;
#5146 = CARTESIAN_POINT ( 'NONE',  ( 27.45766530510195835, -4.728742455708699666, -3.627061608673664672 ) ) ;
#5147 = CARTESIAN_POINT ( 'NONE',  ( -17.83875296969244673, 10.53491135297441161, 15.87472302800564350 ) ) ;
#5148 = SURFACE_STYLE_FILL_AREA ( #6606 ) ;
#5149 = CARTESIAN_POINT ( 'NONE',  ( 30.92509028327567933, -4.310986222078405206, -7.939653947423662039 ) ) ;
#5150 = CARTESIAN_POINT ( 'NONE',  ( 30.81132015408399027, -5.578634341498224458, -3.627061608673668225 ) ) ;
#5151 = ORIENTED_EDGE ( 'NONE', *, *, #16415, .T. ) ;
#5152 =( BOUNDED_CURVE ( )  B_SPLINE_CURVE ( 2, ( #13070, #655, #6177, #15887, #2119, #12892, #3462, #6266, #476 ),
 .UNSPECIFIED., .F., .T. ) 
 B_SPLINE_CURVE_WITH_KNOTS ( ( 3, 2, 2, 2, 3 ),
 ( 0.5192307692307692735, 0.5256410256410256610, 0.5384615384615384359, 0.5512820512820513219, 0.5576923076923077094 ),
 .UNSPECIFIED. ) 
 CURVE ( )  GEOMETRIC_REPRESENTATION_ITEM ( )  RATIONAL_B_SPLINE_CURVE ( ( 0.9330127018922192983, 0.9330127018922198534, 1.000000000000000000, 0.8660254037844387076, 1.000000000000000000, 0.8660254037844387076, 1.000000000000000000, 0.9330127018922194093, 0.9330127018922194093 ) ) 
 REPRESENTATION_ITEM ( '' )  );
#5153 = CARTESIAN_POINT ( 'NONE',  ( 33.95908713831676096, -3.945449517755638791, -3.283357778048664688 ) ) ;
#5154 = AXIS2_PLACEMENT_3D ( 'NONE', #7355, #6053, #15681 ) ;
#5155 = DIRECTION ( 'NONE',  ( 1.000000000000000000, -1.776356839400250780E-14, 0.000000000000000000 ) ) ;
#5156 = EDGE_CURVE ( 'NONE', #5316, #2160, #12674, .T. ) ;
#5157 = VERTEX_POINT ( 'NONE', #15314 ) ;
#5158 = CARTESIAN_POINT ( 'NONE',  ( 30.62726312072365431, -1.838986382273682718, 5.783357778048668685 ) ) ;
#5159 = CARTESIAN_POINT ( 'NONE',  ( 28.88938074516742205, -6.437160617781993999, -4.705209693361168455 ) ) ;
#5160 = DIRECTION ( 'NONE',  ( 0.06446199418653537905, 0.9979201627913403261, 4.248110196704583871E-22 ) ) ;
#5161 = CARTESIAN_POINT ( 'NONE',  ( 26.04410741498555382, -2.380969272135942560, -5.113484796970857893 ) ) ;
#5162 = EDGE_CURVE ( 'NONE', #17459, #5666, #533, .T. ) ;
#5163 = CYLINDRICAL_SURFACE ( 'NONE', #5494, 5.000000000000000000 ) ;
#5164 = AXIS2_PLACEMENT_3D ( 'NONE', #13653, #4135, #13741 ) ;
#5165 = CARTESIAN_POINT ( 'NONE',  ( 2.712778981737816508, -3.052578478158503028, -3.130620751971882054 ) ) ;
#5166 = CARTESIAN_POINT ( 'NONE',  ( 31.63243098167119172, -2.771952051906466874, -8.283357778048658915 ) ) ;
#5167 = ORIENTED_EDGE ( 'NONE', *, *, #1129, .F. ) ;
#5168 = CARTESIAN_POINT ( 'NONE',  ( 23.00000000000000000, -16.21813761408365195, 13.00000000000000355 ) ) ;
#5169 = FACE_OUTER_BOUND ( 'NONE', #11774, .T. ) ;
#5170 = DIRECTION ( 'NONE',  ( 0.000000000000000000, -1.000000000000000000, -0.000000000000000000 ) ) ;
#5171 = CYLINDRICAL_SURFACE ( 'NONE', #6442, 2.749999999999992006 ) ;
#5172 = VERTEX_POINT ( 'NONE', #14135 ) ;
#5173 = VECTOR ( 'NONE', #12021, 1000.000000000000000 ) ;
#5174 = CARTESIAN_POINT ( 'NONE',  ( 26.18945719470476163, -6.341381504099093291, -7.820351782355674963 ) ) ;
#5175 = CARTESIAN_POINT ( 'NONE',  ( 33.60446413004628141, -3.988174587000466342, -3.627061608673664672 ) ) ;
#5176 = AXIS2_PLACEMENT_3D ( 'NONE', #13609, #14460, #6194 ) ;
#5177 = EDGE_CURVE ( 'NONE', #15632, #14031, #14066, .T. ) ;
#5178 = CARTESIAN_POINT ( 'NONE',  ( 31.11087420047036289, -5.742416513891037688, 8.283357778048660691 ) ) ;
#5179 = CARTESIAN_POINT ( 'NONE',  ( -27.68235608956435811, -12.07326681422359194, -13.80428259828453896 ) ) ;
#5180 = B_SPLINE_CURVE_WITH_KNOTS ( 'NONE', 3,
 ( #16151, #16334, #13234, #13424, #8975, #17444, #9328, #4976, #6440, #14518, #12042, #1003, #17629, #14866, #2453, #727, #7624, #10505, #13148, #6252, #5064, #16067, #13329, #17543, #10584, #6961, #5323, #8150, #9575, #13849, #5589, #15301, #4166, #9662, #9410, #11106, #13768, #1347, #6694, #10926, #5676, #6869, #12229, #1534 ),
 .UNSPECIFIED., .F., .F.,
 ( 4, 2, 2, 2, 2, 2, 2, 2, 2, 2, 2, 2, 2, 2, 2, 2, 2, 2, 2, 2, 2, 4 ),
 ( 0.000000000000000000, 0.001235617314710323825, 0.001853425972065488340, 0.002471234629420653289, 0.003706851944130986655, 0.004324660601486156157, 0.004942469258841326527, 0.006178086573551669868, 0.007413703888262013209, 0.008031512545617180976, 0.008649321202972348743, 0.009884938517682682543, 0.01112055583239301808, 0.01235617314710335361, 0.01297398180445852138, 0.01359179046181369088, 0.01482740777652402121, 0.01606302509123435501, 0.01668083374858951584, 0.01729864240594468014, 0.01853425972065500180, 0.01976987703536532692 ),
 .UNSPECIFIED. ) ;
#5181 = ORIENTED_EDGE ( 'NONE', *, *, #6884, .T. ) ;
#5182 = AXIS2_PLACEMENT_3D ( 'NONE', #8361, #13892, #1485 ) ;
#5183 = EDGE_CURVE ( 'NONE', #4257, #2866, #12363, .T. ) ;
#5184 = PLANE ( 'NONE',  #3531 ) ;
#5185 = CARTESIAN_POINT ( 'NONE',  ( 5.781152949374531502, 1.605699403978890993, -2.000000000000000000 ) ) ;
#5186 = CARTESIAN_POINT ( 'NONE',  ( 4.211140560182196957, 2.431303136016537803, -3.445885042887434579 ) ) ;
#5187 = CIRCLE ( 'NONE', #12148, 2.041999999999999815 ) ;
#5188 = CARTESIAN_POINT ( 'NONE',  ( 25.40682704530840397, -3.522014380262483702, -8.283357778048658915 ) ) ;
#5189 = DIRECTION ( 'NONE',  ( 0.000000000000000000, 0.000000000000000000, -1.000000000000000000 ) ) ;
#5190 = CARTESIAN_POINT ( 'NONE',  ( 25.11802603177690330, -19.03270077640483038, 0.5379818257722508434 ) ) ;
#5191 = DIRECTION ( 'NONE',  ( 0.000000000000000000, 0.000000000000000000, -1.000000000000000000 ) ) ;
#5192 = CARTESIAN_POINT ( 'NONE',  ( 27.14244485254070938, -4.766720295129625029, -7.939653947423662039 ) ) ;
#5193 = CARTESIAN_POINT ( 'NONE',  ( 25.92467471225709374, -2.732717170633701453, -7.033357778048658027 ) ) ;
#5194 = CARTESIAN_POINT ( 'NONE',  ( 33.83155592109562804, -6.868441680671474536, 5.783357778048657138 ) ) ;
#5195 = ORIENTED_EDGE ( 'NONE', *, *, #12475, .F. ) ;
#5196 = ORIENTED_EDGE ( 'NONE', *, *, #4091, .F. ) ;
#5197 = VECTOR ( 'NONE', #3608, 1000.000000000000114 ) ;
#5198 = CARTESIAN_POINT ( 'NONE',  ( 31.44176105920648823, -5.502678662656354192, 7.939653947423658487 ) ) ;
#5199 = CARTESIAN_POINT ( 'NONE',  ( -16.79182286896198306, -15.38653328895459893, 16.02976683711036898 ) ) ;
#5200 = DIRECTION ( 'NONE',  ( 0.9928203230275510771, 0.1196152422706609902, 4.006172263299092517E-17 ) ) ;
#5201 = EDGE_LOOP ( 'NONE', ( #14346, #2164, #3184, #8400 ) ) ;
#5202 = FILL_AREA_STYLE_COLOUR ( '', #4423 ) ;
#5203 = CARTESIAN_POINT ( 'NONE',  ( 33.23365877489121090, -6.550928303235100891, -5.783357778048663356 ) ) ;
#5204 = ORIENTED_EDGE ( 'NONE', *, *, #11515, .T. ) ;
#5205 = LINE ( 'NONE', #16125, #1535 ) ;
#5206 =( GEOMETRIC_REPRESENTATION_CONTEXT ( 3 ) GLOBAL_UNCERTAINTY_ASSIGNED_CONTEXT ( ( #3004 ) ) GLOBAL_UNIT_ASSIGNED_CONTEXT ( ( #4939, #2245, #3502 ) ) REPRESENTATION_CONTEXT ( 'NONE', 'WORKASPACE' ) );
#5207 = CARTESIAN_POINT ( 'NONE',  ( 31.24031073583692475, -4.273008382657478954, -3.627061608673664672 ) ) ;
#5208 = ORIENTED_EDGE ( 'NONE', *, *, #4556, .T. ) ;
#5209 = EDGE_CURVE ( 'NONE', #6049, #11429, #13958, .T. ) ;
#5210 = CARTESIAN_POINT ( 'NONE',  ( 30.71189515440122975, -6.854751018602581958, -5.783357778048663356 ) ) ;
#5211 = CARTESIAN_POINT ( 'NONE',  ( -19.43845002722867221, 2.988003976273734263, 0.000000000000000000 ) ) ;
#5212 = DIRECTION ( 'NONE',  ( -1.000000000000000000, 0.000000000000000000, 0.000000000000000000 ) ) ;
#5213 = CARTESIAN_POINT ( 'NONE',  ( 26.47269060886452507, -6.728324053342490174, 4.705209693361160461 ) ) ;
#5214 = AXIS2_PLACEMENT_3D ( 'NONE', #16429, #8170, #13701 ) ;
#5215 = LINE ( 'NONE', #16308, #13101 ) ;
#5216 = CARTESIAN_POINT ( 'NONE',  ( 0.000000000000000000, 0.000000000000000000, 0.000000000000000000 ) ) ;
#5217 = CARTESIAN_POINT ( 'NONE',  ( 32.93470988637010066, -5.949778345213319497, 4.705209693361159573 ) ) ;
#5218 = CARTESIAN_POINT ( 'NONE',  ( 28.52524344760924180, -2.419399995203538101, 4.533357778048667797 ) ) ;
#5219 = EDGE_LOOP ( 'NONE', ( #8639, #7984, #174, #17028 ) ) ;
#5220 = CIRCLE ( 'NONE', #1181, 13.00000000000000178 ) ;
#5221 = VERTEX_POINT ( 'NONE', #8701 ) ;
#5222 = CARTESIAN_POINT ( 'NONE',  ( 31.38469755857769528, -2.374701023479507178, 6.861505862736165362 ) ) ;
#5223 = CARTESIAN_POINT ( 'NONE',  ( 2.500000000000000000, -1.178949249685213863, 2.042000000000001148 ) ) ;
#5224 = CARTESIAN_POINT ( 'NONE',  ( 30.17635249042624679, -2.520282741259753045, 4.705209693361168455 ) ) ;
#5225 = CARTESIAN_POINT ( 'NONE',  ( 33.95908713831673964, -3.945449517755637903, 5.783357778048663356 ) ) ;
#5226 = AXIS2_PLACEMENT_3D ( 'NONE', #17157, #7528, #3267 ) ;
#5227 = CARTESIAN_POINT ( 'NONE',  ( 32.24155699611449677, -1.634298987580965923, 5.783357778048662468 ) ) ;
#5228 = CARTESIAN_POINT ( 'NONE',  ( 30.05329989404488700, -6.934098741245490416, -5.113484796970860558 ) ) ;
#5229 = CARTESIAN_POINT ( 'NONE',  ( 29.77797860222238313, -3.195249460342344250, -3.627061608673662008 ) ) ;
#5230 = CARTESIAN_POINT ( 'NONE',  ( 30.17644170758179101, -4.401183590806859947, 8.283357778048662468 ) ) ;
#5231 = CARTESIAN_POINT ( 'NONE',  ( 33.04340326765378677, -1.875050963503474222, -4.533357778048659803 ) ) ;
#5232 = CARTESIAN_POINT ( 'NONE',  ( 32.00093131988006689, -6.699447617117800569, 5.113484796970852564 ) ) ;
#5233 = ADVANCED_FACE ( 'NONE', ( #177 ), #17055, .F. ) ;
#5234 = CARTESIAN_POINT ( 'NONE',  ( 27.15566825608056689, -6.646038734597135011, -4.705209693361169343 ) ) ;
#5235 = VECTOR ( 'NONE', #14961, 1000.000000000000114 ) ;
#5236 = DIRECTION ( 'NONE',  ( 0.9928203230275512992, 0.1196152422706587698, 0.000000000000000000 ) ) ;
#5237 = ADVANCED_FACE ( 'NONE', ( #8796, #4343 ), #3626, .F. ) ;
#5238 = VECTOR ( 'NONE', #17183, 1000.000000000000000 ) ;
#5239 = CARTESIAN_POINT ( 'NONE',  ( 30.29464937815318493, -4.386941900920275472, -7.939653947423662039 ) ) ;
#5240 = CARTESIAN_POINT ( 'NONE',  ( 32.93470988637010066, -5.949778345213319497, -6.861505862736167138 ) ) ;
#5241 = CARTESIAN_POINT ( 'NONE',  ( 26.01652455409633902, -4.902371455920928156, -5.783357778048663356 ) ) ;
#5242 = VECTOR ( 'NONE', #1265, 1000.000000000000000 ) ;
#5243 = CARTESIAN_POINT ( 'NONE',  ( 25.92467471225709374, -2.732717170633701453, 4.533357778048667797 ) ) ;
#5244 = ORIENTED_EDGE ( 'NONE', *, *, #15743, .F. ) ;
#5245 = VERTEX_POINT ( 'NONE', #2362 ) ;
#5246 = CARTESIAN_POINT ( 'NONE',  ( 32.54503264317084188, -5.369756224683081669, 7.939653947423658487 ) ) ;
#5247 = VECTOR ( 'NONE', #14814, 1000.000000000000000 ) ;
#5248 = CARTESIAN_POINT ( 'NONE',  ( 27.62849893492243325, -6.589071975465733644, -4.705209693361168455 ) ) ;
#5249 = CARTESIAN_POINT ( 'NONE',  ( 28.20260476654369697, -6.819712339336020612, 4.533357778048659803 ) ) ;
#5250 = CARTESIAN_POINT ( 'NONE',  ( 26.83664947211162399, -6.984282976826746037, -4.533357778048668685 ) ) ;
#5251 = CARTESIAN_POINT ( 'NONE',  ( 26.31556265977298992, -7.384422263489805793, -5.783357778048663356 ) ) ;
#5252 = AXIS2_PLACEMENT_3D ( 'NONE', #1365, #6890, #12419 ) ;
#5253 = DIRECTION ( 'NONE',  ( 1.000000000000000000, 0.000000000000000000, 0.000000000000000000 ) ) ;
#5254 = CARTESIAN_POINT ( 'NONE',  ( 30.37154917142620292, -2.923863409590206519, -8.283357778048658915 ) ) ;
#5255 =( BOUNDED_CURVE ( )  B_SPLINE_CURVE ( 2, ( #15451, #3034, #14089, #1676, #9990, #7210, #15535, #12722, #10179 ),
 .UNSPECIFIED., .F., .T. ) 
 B_SPLINE_CURVE_WITH_KNOTS ( ( 3, 2, 2, 2, 3 ),
 ( 0.5192307692307692735, 0.5256410256410256610, 0.5384615384615384359, 0.5512820512820513219, 0.5576923076923077094 ),
 .UNSPECIFIED. ) 
 CURVE ( )  GEOMETRIC_REPRESENTATION_ITEM ( )  RATIONAL_B_SPLINE_CURVE ( ( 0.9330127018922192983, 0.9330127018922198534, 1.000000000000000000, 0.8660254037844387076, 1.000000000000000000, 0.8660254037844387076, 1.000000000000000000, 0.9330127018922194093, 0.9330127018922194093 ) ) 
 REPRESENTATION_ITEM ( '' )  );
#5256 = EDGE_CURVE ( 'NONE', #1670, #761, #1101, .T. ) ;
#5257 = VERTEX_POINT ( 'NONE', #13044 ) ;
#5258 = CARTESIAN_POINT ( 'NONE',  ( 33.19286683830256379, -2.783822866615540903, -7.939653947423660263 ) ) ;
#5259 = CARTESIAN_POINT ( 'NONE',  ( 26.24651417059167358, -6.811311830135031720, -4.396611942026659392 ) ) ;
#5260 = DIRECTION ( 'NONE',  ( -1.000000000000000000, -0.000000000000000000, -0.000000000000000000 ) ) ;
#5261 = DIRECTION ( 'NONE',  ( -0.9979201627913402151, 0.06446199418653550395, 5.311609029246448998E-22 ) ) ;
#5262 = APPLICATION_CONTEXT ( 'automotive_design' ) ;
#5263 = DIRECTION ( 'NONE',  ( -0.000000000000000000, 1.000000000000000000, -0.000000000000000000 ) ) ;
#5264 = CARTESIAN_POINT ( 'NONE',  ( 33.14902674121363901, -1.535163666906202318, -5.783357778048658915 ) ) ;
#5265 = EDGE_CURVE ( 'NONE', #9127, #13220, #1997, .T. ) ;
#5266 = MANIFOLD_SOLID_BREP ( '<Caliper Body Half>-<Thread1>', #4921 ) ;
#5267 = AXIS2_PLACEMENT_3D ( 'NONE', #9775, #6898, #16518 ) ;
#5268 = VERTEX_POINT ( 'NONE', #9228 ) ;
#5269 = DIRECTION ( 'NONE',  ( 1.000000000000000000, 0.000000000000000000, 0.000000000000000000 ) ) ;
#5270 = ORIENTED_EDGE ( 'NONE', *, *, #13658, .F. ) ;
#5271 = CARTESIAN_POINT ( 'NONE',  ( -29.03633718710667466, -14.58471626061076520, -13.43311195353574305 ) ) ;
#5272 = ORIENTED_EDGE ( 'NONE', *, *, #265, .F. ) ;
#5273 = SURFACE_SIDE_STYLE ('',( #12169 ) ) ;
#5274 = VECTOR ( 'NONE', #14997, 1000.000000000000227 ) ;
#5275 = CARTESIAN_POINT ( 'NONE',  ( 30.91186687973582536, -2.431667782610909434, -4.705209693361160461 ) ) ;
#5276 = DIRECTION ( 'NONE',  ( -1.000000000000000000, 0.000000000000000000, 0.000000000000000000 ) ) ;
#5277 = EDGE_CURVE ( 'NONE', #4804, #825, #4857, .T. ) ;
#5278 =( BOUNDED_SURFACE ( )  B_SPLINE_SURFACE ( 1, 2, ( 
 ( #5930, #14193, #17021, #11644, #11454, #8568, #14294, #17212, #11362, #14019, #12918, #4665, #11258, #1881, #10193, #8845, #15465, #6017, #1688, #7408, #503, #3048, #10096, #7223, #7485, #12735, #332, #3318, #15645, #1603, #16932, #10004, #17113, #9821, #3131, #14381, #15371, #2954, #17399, #14654, #17499, #3762, #7579, #771, #15918, #12004, #13107, #2237, #4929, #7749, #10624, #11728, #14741, #2328, #16197, #9284, #14825, #9116, #13471, #10364, #685, #860, #3493, #13280, #2151, #2057, #9196, #6299, #6393, #12084, #15827, #6211, #17300, #11910, #5024, #7670, #5105, #7847, #13194, #10546, #4838, #3400, #10461, #7934, #2413, #1044, #16110, #10278, #3671, #14574, #13373, #8930, #11820, #6564, #14473, #16022, #956, #9024, #3593, #6489, #17585, #4752, #12356, #17757, #2835, #3855, #16629, #15176, #6650, #6831, #2757, #4206, #17924, #12180, #8276, #9538, #13636, #13807, #1125, #3937, #5365, #9624, #1394, #11068, #5456, #10975, #5192, #6915, #15085, #5282, #1488, #8363, #12448, #10712, #8011, #10799, #16537, #35, #7016, #5544, #9706, #4115, #13894, #1309, #10885, #15256, #16454, #16374, #14906, #8102, #1226, #2668, #8198, #17669, #16285 ),
 ( #17846, #13724, #9366, #9452, #2489, #13550, #14989, #2575, #6741, #4022, #12277, #212, #2929, #8640, #5720, #15529, #9893, #9798, #16998, #14081, #305, #16718, #8550, #4552, #14360, #16815, #4469, #3111, #1581, #10074, #15349, #5996, #15621, #14170, #3199, #11238, #8740, #1945, #16913, #15445, #403, #8828, #8464, #11434, #123, #4380, #12540, #3026, #11337, #1667, #7115, #7203, #13997, #12628, #7388, #9982, #1760, #12712, #5815, #1859, #7291, #10172, #12809, #5632, #11148, #5909, #14270, #12902, #486, #11523, #17091, #4646, #15723, #3298, #4289, #6093, #7652, #10609, #17568, #5088, #17377, #12989, #9095, #17280, #7731, #11622, #10345, #9263, #17187, #2131, #10439, #3381, #8914, #2218, #4733, #16176, #13258, #7557, #3738, #10257, #6471, #5004, #14451, #14637, #10529, #11985, #840, #2032, #16090, #4911, #3472, #3657, #13083, #11709, #13175, #17473, #9178, #934, #6369, #11892, #574, #14722, #15999, #664, #14808, #7465, #2306, #15807, #6187, #4816, #7824, #13355, #15898, #9002, #14550, #751, #6278, #11799, #3572, #17908, #8086, #9352, #17651, #10782, #16360, #5347, #17828, #1294, #15159, #10689, #10868, #14890, #5174, #6633, #2476 ) ),
 .UNSPECIFIED., .F., .F., .T. ) 
 B_SPLINE_SURFACE_WITH_KNOTS ( ( 2, 2 ),
 ( 3, 2, 2, 2, 2, 2, 2, 2, 2, 2, 2, 2, 2, 2, 2, 2, 2, 2, 2, 2, 2, 2, 2, 2, 2, 2, 2, 2, 2, 2, 2, 2, 2, 2, 2, 2, 2, 2, 2, 2, 2, 2, 2, 2, 2, 2, 2, 2, 2, 2, 2, 2, 2, 2, 2, 2, 2, 2, 2, 2, 2, 2, 2, 2, 2, 2, 2, 2, 2, 2, 2, 2, 2, 2, 2, 2, 2, 3 ),
 ( 0.000000000000000000, 1.000000000000000000 ),
 ( 0.000000000000000000, 0.01282051282051282007, 0.02564102564102564014, 0.03846153846153846367, 0.05128205128205128027, 0.06410256410256409687, 0.07692307692307692735, 0.08974358974358974395, 0.1025641025641025605, 0.1153846153846153910, 0.1282051282051281937, 0.1410256410256410242, 0.1538461538461538547, 0.1666666666666666574, 0.1794871794871794879, 0.1923076923076923184, 0.2051282051282051211, 0.2179487179487179516, 0.2307692307692307820, 0.2435897435897435848, 0.2564102564102563875, 0.2692307692307692180, 0.2820512820512820484, 0.2948717948717948789, 0.3076923076923077094, 0.3205128205128205399, 0.3333333333333333148, 0.3461538461538461453, 0.3589743589743589758, 0.3717948717948718063, 0.3846153846153846367, 0.3974358974358974117, 0.4102564102564102422, 0.4230769230769230727, 0.4358974358974359031, 0.4487179487179487336, 0.4615384615384615641, 0.4743589743589743390, 0.4871794871794871695, 0.5000000000000000000, 0.5128205128205127750, 0.5256410256410256610, 0.5384615384615384359, 0.5512820512820513219, 0.5641025641025640969, 0.5769230769230768718, 0.5897435897435897578, 0.6025641025641025328, 0.6153846153846154188, 0.6282051282051281937, 0.6410256410256410797, 0.6538461538461538547, 0.6666666666666666297, 0.6794871794871795156, 0.6923076923076922906, 0.7051282051282051766, 0.7179487179487179516, 0.7307692307692307265, 0.7435897435897436125, 0.7564102564102563875, 0.7692307692307692735, 0.7820512820512820484, 0.7948717948717948234, 0.8076923076923077094, 0.8205128205128204844, 0.8333333333333333703, 0.8461538461538461453, 0.8589743589743589203, 0.8717948717948718063, 0.8846153846153845812, 0.8974358974358974672, 0.9102564102564102422, 0.9230769230769231282, 0.9358974358974359031, 0.9487179487179486781, 0.9615384615384615641, 0.9690837477411259338, 0.9787745852185372186 ),
 .UNSPECIFIED. ) 
 GEOMETRIC_REPRESENTATION_ITEM ( )  RATIONAL_B_SPLINE_SURFACE ( (
 ( 1.000000000000000000, 0.8660254037844387076, 1.000000000000000000, 0.8660254037844387076, 1.000000000000000000, 0.8660254037844387076, 1.000000000000000000, 0.8660254037844387076, 1.000000000000000000, 0.8660254037844387076, 1.000000000000000000, 0.8660254037844387076, 1.000000000000000000, 0.8660254037844387076, 1.000000000000000000, 0.8660254037844387076, 1.000000000000000000, 0.8660254037844387076, 1.000000000000000000, 0.8660254037844387076, 1.000000000000000000, 0.8660254037844387076, 1.000000000000000000, 0.8660254037844387076, 1.000000000000000000, 0.8660254037844387076, 1.000000000000000000, 0.8660254037844387076, 1.000000000000000000, 0.8660254037844387076, 1.000000000000000000, 0.8660254037844387076, 1.000000000000000000, 0.8660254037844387076, 1.000000000000000000, 0.8660254037844387076, 1.000000000000000000, 0.8660254037844387076, 1.000000000000000000, 0.8660254037844387076, 1.000000000000000000, 0.8660254037844387076, 1.000000000000000000, 0.8660254037844387076, 1.000000000000000000, 0.8660254037844387076, 1.000000000000000000, 0.8660254037844387076, 1.000000000000000000, 0.8660254037844387076, 1.000000000000000000, 0.8660254037844387076, 1.000000000000000000, 0.8660254037844387076, 1.000000000000000000, 0.8660254037844387076, 1.000000000000000000, 0.8660254037844387076, 1.000000000000000000, 0.8660254037844387076, 1.000000000000000000, 0.8660254037844387076, 1.000000000000000000, 0.8660254037844387076, 1.000000000000000000, 0.8660254037844387076, 1.000000000000000000, 0.8660254037844387076, 1.000000000000000000, 0.8660254037844387076, 1.000000000000000000, 0.8660254037844387076, 1.000000000000000000, 0.8660254037844387076, 1.000000000000000000, 0.8660254037844387076, 1.000000000000000000, 0.8660254037844387076, 1.000000000000000000, 0.8660254037844387076, 1.000000000000000000, 0.8660254037844387076, 1.000000000000000000, 0.8660254037844387076, 1.000000000000000000, 0.8660254037844387076, 1.000000000000000000, 0.8660254037844387076, 1.000000000000000000, 0.8660254037844387076, 1.000000000000000000, 0.8660254037844387076, 1.000000000000000000, 0.8660254037844387076, 1.000000000000000000, 0.8660254037844387076, 1.000000000000000000, 0.8660254037844387076, 1.000000000000000000, 0.8660254037844387076, 1.000000000000000000, 0.8660254037844387076, 1.000000000000000000, 0.8660254037844387076, 1.000000000000000000, 0.8660254037844387076, 1.000000000000000000, 0.8660254037844387076, 1.000000000000000000, 0.8660254037844387076, 1.000000000000000000, 0.8660254037844387076, 1.000000000000000000, 0.8660254037844387076, 1.000000000000000000, 0.8660254037844387076, 1.000000000000000000, 0.8660254037844387076, 1.000000000000000000, 0.8660254037844387076, 1.000000000000000000, 0.8660254037844387076, 1.000000000000000000, 0.8660254037844387076, 1.000000000000000000, 0.8660254037844387076, 1.000000000000000000, 0.8660254037844387076, 1.000000000000000000, 0.8660254037844387076, 1.000000000000000000, 0.8660254037844387076, 1.000000000000000000, 0.8660254037844387076, 1.000000000000000000, 0.8660254037844387076, 1.000000000000000000, 0.8660254037844387076, 1.000000000000000000, 0.8660254037844387076, 1.000000000000000000, 0.8660254037844387076, 1.000000000000000000, 0.8660254037844387076, 1.000000000000000000, 0.8660254037844387076, 1.000000000000000000, 0.8660254037844387076, 1.000000000000000000, 0.8660254037844387076, 1.000000000000000000, 0.9211516195580409239, 0.9351128802560608744, 0.9351128802560608744, 0.9351128802560608744),
 ( 1.000000000000000000, 0.8660254037844387076, 1.000000000000000000, 0.8660254037844387076, 1.000000000000000000, 0.8660254037844387076, 1.000000000000000000, 0.8660254037844387076, 1.000000000000000000, 0.8660254037844387076, 1.000000000000000000, 0.8660254037844387076, 1.000000000000000000, 0.8660254037844387076, 1.000000000000000000, 0.8660254037844387076, 1.000000000000000000, 0.8660254037844387076, 1.000000000000000000, 0.8660254037844387076, 1.000000000000000000, 0.8660254037844387076, 1.000000000000000000, 0.8660254037844387076, 1.000000000000000000, 0.8660254037844387076, 1.000000000000000000, 0.8660254037844387076, 1.000000000000000000, 0.8660254037844387076, 1.000000000000000000, 0.8660254037844387076, 1.000000000000000000, 0.8660254037844387076, 1.000000000000000000, 0.8660254037844387076, 1.000000000000000000, 0.8660254037844387076, 1.000000000000000000, 0.8660254037844387076, 1.000000000000000000, 0.8660254037844387076, 1.000000000000000000, 0.8660254037844387076, 1.000000000000000000, 0.8660254037844387076, 1.000000000000000000, 0.8660254037844387076, 1.000000000000000000, 0.8660254037844387076, 1.000000000000000000, 0.8660254037844387076, 1.000000000000000000, 0.8660254037844387076, 1.000000000000000000, 0.8660254037844387076, 1.000000000000000000, 0.8660254037844387076, 1.000000000000000000, 0.8660254037844387076, 1.000000000000000000, 0.8660254037844387076, 1.000000000000000000, 0.8660254037844387076, 1.000000000000000000, 0.8660254037844387076, 1.000000000000000000, 0.8660254037844387076, 1.000000000000000000, 0.8660254037844387076, 1.000000000000000000, 0.8660254037844387076, 1.000000000000000000, 0.8660254037844387076, 1.000000000000000000, 0.8660254037844387076, 1.000000000000000000, 0.8660254037844387076, 1.000000000000000000, 0.8660254037844387076, 1.000000000000000000, 0.8660254037844387076, 1.000000000000000000, 0.8660254037844387076, 1.000000000000000000, 0.8660254037844387076, 1.000000000000000000, 0.8660254037844387076, 1.000000000000000000, 0.8660254037844387076, 1.000000000000000000, 0.8660254037844387076, 1.000000000000000000, 0.8660254037844387076, 1.000000000000000000, 0.8660254037844387076, 1.000000000000000000, 0.8660254037844387076, 1.000000000000000000, 0.8660254037844387076, 1.000000000000000000, 0.8660254037844387076, 1.000000000000000000, 0.8660254037844387076, 1.000000000000000000, 0.8660254037844387076, 1.000000000000000000, 0.8660254037844387076, 1.000000000000000000, 0.8660254037844387076, 1.000000000000000000, 0.8660254037844387076, 1.000000000000000000, 0.8660254037844387076, 1.000000000000000000, 0.8660254037844387076, 1.000000000000000000, 0.8660254037844387076, 1.000000000000000000, 0.8660254037844387076, 1.000000000000000000, 0.8660254037844387076, 1.000000000000000000, 0.8660254037844387076, 1.000000000000000000, 0.8660254037844387076, 1.000000000000000000, 0.8660254037844387076, 1.000000000000000000, 0.8660254037844387076, 1.000000000000000000, 0.8660254037844387076, 1.000000000000000000, 0.8660254037844387076, 1.000000000000000000, 0.8660254037844387076, 1.000000000000000000, 0.8660254037844387076, 1.000000000000000000, 0.8660254037844387076, 1.000000000000000000, 0.8660254037844387076, 1.000000000000000000, 0.8660254037844387076, 1.000000000000000000, 0.8660254037844387076, 1.000000000000000000, 0.8660254037844387076, 1.000000000000000000, 0.8660254037844387076, 1.000000000000000000, 0.9211516195580409239, 0.9351128802560608744, 0.9351128802560608744, 0.9351128802560608744) ) ) 
 REPRESENTATION_ITEM ( '' )  SURFACE ( )  );
#5279 = CARTESIAN_POINT ( 'NONE',  ( 26.78782184427022983, -4.809445364374452581, -8.283357778048662468 ) ) ;
#5280 = CARTESIAN_POINT ( 'NONE',  ( -35.46635924378174565, -16.45598204045937152, 11.37070560279562059 ) ) ;
#5281 = DIRECTION ( 'NONE',  ( -0.000000000000000000, -0.000000000000000000, -1.000000000000000000 ) ) ;
#5282 = CARTESIAN_POINT ( 'NONE',  ( 27.28266178881210280, -7.257709054644824853, -5.783357778048669573 ) ) ;
#5283 = DIRECTION ( 'NONE',  ( -0.000000000000000000, -0.000000000000000000, 1.000000000000000000 ) ) ;
#5284 = CARTESIAN_POINT ( 'NONE',  ( 31.17093069310692499, -6.462087684996337345, 7.033357778048657138 ) ) ;
#5285 = VERTEX_POINT ( 'NONE', #17435 ) ;
#5286 = EDGE_CURVE ( 'NONE', #16203, #2633, #15924, .T. ) ;
#5287 = CARTESIAN_POINT ( 'NONE',  ( 31.03886041246737548, -3.043338102658604161, 7.939653947423664704 ) ) ;
#5288 = LINE ( 'NONE', #8109, #7548 ) ;
#5289 = CARTESIAN_POINT ( 'NONE',  ( 23.43992347230441453, -22.46596520570847844, 14.83047979245100656 ) ) ;
#5290 = VERTEX_POINT ( 'NONE', #8880 ) ;
#5291 = LINE ( 'NONE', #16122, #3280 ) ;
#5292 = LINE ( 'NONE', #10811, #3182 ) ;
#5293 = CARTESIAN_POINT ( 'NONE',  ( 0.000000000000000000, 0.000000000000000000, -2.000000000000000000 ) ) ;
#5294 = CARTESIAN_POINT ( 'NONE',  ( 30.18087924896149588, -5.654590020340094725, -3.627061608673668225 ) ) ;
#5295 = EDGE_LOOP ( 'NONE', ( #13952, #9503, #5995, #6493, #2922 ) ) ;
#5296 = EDGE_CURVE ( 'NONE', #15182, #8284, #3132, .T. ) ;
#5297 = CARTESIAN_POINT ( 'NONE',  ( 25.71748644841968456, -2.420320648352046078, -5.783357778048663356 ) ) ;
#5298 = CARTESIAN_POINT ( 'NONE',  ( 25.11802603177690330, -19.03270077640482683, -10.53798182577225084 ) ) ;
#5299 = DIRECTION ( 'NONE',  ( 0.000000000000000000, 0.000000000000000000, -1.000000000000000000 ) ) ;
#5300 = CARTESIAN_POINT ( 'NONE',  ( 33.20550441965735899, -6.554320347036139971, 6.453230759126467042 ) ) ;
#5301 = ORIENTED_EDGE ( 'NONE', *, *, #11786, .F. ) ;
#5302 = CARTESIAN_POINT ( 'NONE',  ( 27.49697864365563760, -2.843094376337701679, 4.705209693361167567 ) ) ;
#5303 = DIRECTION ( 'NONE',  ( 1.000000000000000000, 0.000000000000000000, 0.000000000000000000 ) ) ;
#5304 = CARTESIAN_POINT ( 'NONE',  ( 32.50309786422735669, -5.574681056656013212, 3.283357778048663356 ) ) ;
#5305 = CARTESIAN_POINT ( 'NONE',  ( 32.30426898124760982, -6.025734024055190652, 4.705209693361159573 ) ) ;
#5306 = ORIENTED_EDGE ( 'NONE', *, *, #12713, .T. ) ;
#5307 = CARTESIAN_POINT ( 'NONE',  ( 29.49727470010032704, -7.390636972501882340, 5.783357778048657138 ) ) ;
#5308 = ORIENTED_EDGE ( 'NONE', *, *, #8547, .F. ) ;
#5309 = EDGE_LOOP ( 'NONE', ( #13206, #9388 ) ) ;
#5310 = EDGE_CURVE ( 'NONE', #1421, #7830, #14508, .T. ) ;
#5311 = CARTESIAN_POINT ( 'NONE',  ( 30.90769699326644826, -6.820963901304073929, 5.783357778048658027 ) ) ;
#5312 = CARTESIAN_POINT ( 'NONE',  ( 0.000000000000000000, 0.000000000000000000, -2.000000000000000000 ) ) ;
#5313 = CARTESIAN_POINT ( 'NONE',  ( 28.89355063163679915, -2.047864499088824175, 5.783357778048668685 ) ) ;
#5314 = CARTESIAN_POINT ( 'NONE',  ( 29.82675284572052732, -1.925235199084722959, 6.453230759126469707 ) ) ;
#5315 = CARTESIAN_POINT ( 'NONE',  ( 25.29083129957448151, -4.989803161779970964, 5.783357778048662468 ) ) ;
#5316 = VERTEX_POINT ( 'NONE', #15863 ) ;
#5317 = CARTESIAN_POINT ( 'NONE',  ( 27.27683486999669427, -2.232449958253242883, -5.783357778048658027 ) ) ;
#5318 = FACE_BOUND ( 'NONE', #17618, .T. ) ;
#5319 = LINE ( 'NONE', #3806, #12197 ) ;
#5320 = CARTESIAN_POINT ( 'NONE',  ( 28.56587103547553852, -2.077146556768465047, -5.113484796970851676 ) ) ;
#5321 = DIRECTION ( 'NONE',  ( -0.8660254037844381525, -0.5000000000000007772, 0.000000000000000000 ) ) ;
#5322 = CARTESIAN_POINT ( 'NONE',  ( 29.20802265909081896, -15.38590642643731066, -13.38453386482100171 ) ) ;
#5323 = CARTESIAN_POINT ( 'NONE',  ( 25.01746843935482190, -10.28886876799018246, 14.47312570928799680 ) ) ;
#5324 = CARTESIAN_POINT ( 'NONE',  ( 32.70264286945147347, -5.350767304972614546, -3.627061608673668225 ) ) ;
#5325 = CARTESIAN_POINT ( 'NONE',  ( 29.77797860222238313, -3.195249460342344250, -3.627061608673662008 ) ) ;
#5326 = DIRECTION ( 'NONE',  ( 0.9928203230275510771, 0.1196152422706614621, -0.000000000000000000 ) ) ;
#5327 = CARTESIAN_POINT ( 'NONE',  ( 33.40745134805642635, -4.011910736534825439, -3.283357778048664688 ) ) ;
#5328 = PRODUCT_DEFINITION_SHAPE ( 'NONE', 'NONE',  #17980 ) ;
#5329 = ORIENTED_EDGE ( 'NONE', *, *, #13805, .T. ) ;
#5330 = EDGE_CURVE ( 'NONE', #1198, #10066, #8966, .T. ) ;
#5331 = CARTESIAN_POINT ( 'NONE',  ( 31.71314141467879111, -4.216041623526076698, 7.939653947423662039 ) ) ;
#5332 = CARTESIAN_POINT ( 'NONE',  ( 28.86293393808771057, -2.678523738846987357, -4.705209693361161349 ) ) ;
#5333 = CARTESIAN_POINT ( 'NONE',  ( 9.458171371211037126, 3.728626979641400219, -2.666481567098320848 ) ) ;
#5334 = LINE ( 'NONE', #16251, #10441 ) ;
#5335 = LINE ( 'NONE', #10771, #11308 ) ;
#5336 = CARTESIAN_POINT ( 'NONE',  ( 16.75000000000000000, -16.21813761408365195, 16.03574476417184513 ) ) ;
#5337 = DIRECTION ( 'NONE',  ( 0.000000000000000000, 1.000000000000000000, -0.000000000000000000 ) ) ;
#5338 = UNCERTAINTY_MEASURE_WITH_UNIT (LENGTH_MEASURE( 1.000000000000000082E-05 ), #12550, 'distance_accuracy_value', 'NONE');
#5339 = B_SPLINE_CURVE_WITH_KNOTS ( 'NONE', 3,
 ( #17440, #14419, #11957, #15778, #2097, #4972 ),
 .UNSPECIFIED., .F., .F.,
 ( 4, 2, 4 ),
 ( 0.000000000000000000, 0.0002095117440854745035, 0.0004190234881709490071 ),
 .UNSPECIFIED. ) ;
#5340 = CARTESIAN_POINT ( 'NONE',  ( 28.91555989733679866, -4.553094948490599592, -3.283357778048664688 ) ) ;
#5341 = ORIENTED_EDGE ( 'NONE', *, *, #4529, .T. ) ;
#5342 = VERTEX_POINT ( 'NONE', #4875 ) ;
#5343 = CARTESIAN_POINT ( 'NONE',  ( 32.16857880351144416, -6.669052543620333395, -5.783357778048668685 ) ) ;
#5344 = SURFACE_STYLE_USAGE ( .BOTH. , #12609 ) ;
#5345 = CARTESIAN_POINT ( 'NONE',  ( 30.33776104811456165, -2.201027418740610919, -7.033357778048658027 ) ) ;
#5346 = CARTESIAN_POINT ( 'NONE',  ( 0.6810530063609926410, 4.461079733298231709, -3.298443181296264459 ) ) ;
#5347 = CARTESIAN_POINT ( 'NONE',  ( 26.16860980394290692, -3.430234601869349920, -3.283357778048662023 ) ) ;
#5348 = CARTESIAN_POINT ( 'NONE',  ( 29.19137779418881351, -4.519864338893556877, -3.627061608673664672 ) ) ;
#5349 = MANIFOLD_SOLID_BREP ( 'TorqueElement', #17724 ) ;
#5350 = EDGE_CURVE ( 'NONE', #1158, #3640, #14742, .T. ) ;
#5351 = EDGE_CURVE ( 'NONE', #9800, #15040, #17670, .T. ) ;
#5352 = CARTESIAN_POINT ( 'NONE',  ( -9.099998387031003944, -19.29508120620799616, 16.81964500401478091 ) ) ;
#5353 = ORIENTED_EDGE ( 'NONE', *, *, #12316, .T. ) ;
#5354 = COLOUR_RGB ( '', 0.66274510, 0.83137255, 0.94901961) ;
#5355 = FACE_OUTER_BOUND ( 'NONE', #2888, .T. ) ;
#5356 = ORIENTED_EDGE ( 'NONE', *, *, #7800, .F. ) ;
#5357 = CARTESIAN_POINT ( 'NONE',  ( 28.51709679197738723, -3.347160818026084339, -3.627061608673662008 ) ) ;
#5358 = EDGE_LOOP ( 'NONE', ( #15703, #3326 ) ) ;
#5359 = DIRECTION ( 'NONE',  ( 0.000000000000000000, 0.000000000000000000, 1.000000000000000000 ) ) ;
#5360 = VERTEX_POINT ( 'NONE', #10747 ) ;
#5361 = ORIENTED_EDGE ( 'NONE', *, *, #1378, .T. ) ;
#5362 = CARTESIAN_POINT ( 'NONE',  ( 32.77257290155422709, -2.834459985843461816, -3.627061608673662896 ) ) ;
#5363 = DIRECTION ( 'NONE',  ( 0.000000000000000000, 0.000000000000000000, 1.000000000000000000 ) ) ;
#5364 = CARTESIAN_POINT ( 'NONE',  ( 3.999999999999999556, 0.8228621380349563363, -3.130611579770401498 ) ) ;
#5365 = CARTESIAN_POINT ( 'NONE',  ( 27.45766530510195835, -4.728742455708699666, -3.627061608673664672 ) ) ;
#5366 =( GEOMETRIC_REPRESENTATION_CONTEXT ( 3 ) GLOBAL_UNCERTAINTY_ASSIGNED_CONTEXT ( ( #12292 ) ) GLOBAL_UNIT_ASSIGNED_CONTEXT ( ( #979, #6505, #17522 ) ) REPRESENTATION_CONTEXT ( 'NONE', 'WORKASPACE' ) );
#5367 = DIRECTION ( 'NONE',  ( 0.9928203230275510771, 0.1196152422706609902, 4.006172263299092517E-17 ) ) ;
#5368 = EDGE_LOOP ( 'NONE', ( #14706, #14095, #4250, #14788 ) ) ;
#5369 = ADVANCED_FACE ( 'NONE', ( #14857 ), #13500, .T. ) ;
#5370 = CARTESIAN_POINT ( 'NONE',  ( 29.65098506949083301, -2.583579140294649523, 6.861505862736166250 ) ) ;
#5371 = CARTESIAN_POINT ( 'NONE',  ( -17.71052479140136526, -12.88256812061772116, 15.89289657457836746 ) ) ;
#5372 = DIRECTION ( 'NONE',  ( -0.000000000000000000, -0.000000000000000000, -1.000000000000000000 ) ) ;
#5373 = ORIENTED_EDGE ( 'NONE', *, *, #17531, .F. ) ;
#5374 = LINE ( 'NONE', #10809, #16027 ) ;
#5375 = ORIENTED_EDGE ( 'NONE', *, *, #14298, .F. ) ;
#5376 = DIRECTION ( 'NONE',  ( 1.000000000000000000, 0.000000000000000000, 0.000000000000000000 ) ) ;
#5377 =( BOUNDED_CURVE ( )  B_SPLINE_CURVE ( 2, ( #9835, #11009, #1616, #1525, #3059, #7056, #5667, #2970, #1702 ),
 .UNSPECIFIED., .F., .T. ) 
 B_SPLINE_CURVE_WITH_KNOTS ( ( 3, 2, 2, 2, 3 ),
 ( 0.3269230769230769273, 0.3333333333333333148, 0.3461538461538461453, 0.3589743589743589758, 0.3653846153846154188 ),
 .UNSPECIFIED. ) 
 CURVE ( )  GEOMETRIC_REPRESENTATION_ITEM ( )  RATIONAL_B_SPLINE_CURVE ( ( 0.9330127018922194093, 0.9330127018922194093, 1.000000000000000000, 0.8660254037844387076, 1.000000000000000000, 0.8660254037844387076, 1.000000000000000000, 0.9330127018922190762, 0.9330127018922194093 ) ) 
 REPRESENTATION_ITEM ( '' )  );
#5378 = ORIENTED_EDGE ( 'NONE', *, *, #15431, .T. ) ;
#5379 = ORIENTED_EDGE ( 'NONE', *, *, #7811, .F. ) ;
#5380 = LINE ( 'NONE', #3868, #6161 ) ;
#5381 = CARTESIAN_POINT ( 'NONE',  ( 29.54591158530375239, -2.596238420101622868, -6.861505862736158257 ) ) ;
#5382 = PRODUCT_DEFINITION_CONTEXT ( 'detailed design', #4243, 'design' ) ;
#5383 = CARTESIAN_POINT ( 'NONE',  ( 30.69058026372202974, -5.793053633118939061, -8.283357778048664244 ) ) ;
#5384 = FACE_OUTER_BOUND ( 'NONE', #148, .T. ) ;
#5385 = CARTESIAN_POINT ( 'NONE',  ( 1.296864337298335788E-21, -1.182044466681725685E-21, 6.899999999999998579 ) ) ;
#5386 = CARTESIAN_POINT ( 'NONE',  ( 29.79859849048667897, -1.928627242885762705, -5.783357778048664244 ) ) ;
#5387 = CARTESIAN_POINT ( 'NONE',  ( 30.65370992780335868, -5.597623261208691581, 7.939653947423658487 ) ) ;
#5388 = FACE_OUTER_BOUND ( 'NONE', #9335, .T. ) ;
#5389 = CARTESIAN_POINT ( 'NONE',  ( 32.26287188679368256, -2.695996373064596607, 3.283357778048666464 ) ) ;
#5390 = CARTESIAN_POINT ( 'NONE',  ( -16.75000000000000000, -16.21813761408365195, 16.03574476417183448 ) ) ;
#5391 = ORIENTED_EDGE ( 'NONE', *, *, #13189, .T. ) ;
#5392 = EDGE_CURVE ( 'NONE', #16872, #7076, #2563, .T. ) ;
#5393 = ORIENTED_EDGE ( 'NONE', *, *, #16812, .T. ) ;
#5394 = CARTESIAN_POINT ( 'NONE',  ( 31.88814493096863956, -1.687075024589942851, 5.783357778048668685 ) ) ;
#5395 = CARTESIAN_POINT ( 'NONE',  ( 8.632250723006720250, -18.84644399697197770, 13.00000000000000178 ) ) ;
#5396 = ORIENTED_EDGE ( 'NONE', *, *, #10977, .F. ) ;
#5397 = CARTESIAN_POINT ( 'NONE',  ( 29.54591158530375239, -2.596238420101622868, 4.705209693361168455 ) ) ;
#5398 = TOROIDAL_SURFACE ( 'NONE', #864, 10.40000000000000036, 0.9000000000000003553 ) ;
#5399 = CARTESIAN_POINT ( 'NONE',  ( 31.00199007654869732, -2.847907730748336697, -8.283357778048660691 ) ) ;
#5400 = CYLINDRICAL_SURFACE ( 'NONE', #12429, 2.500000000000001776 ) ;
#5401 = CARTESIAN_POINT ( 'NONE',  ( 28.76917853929504432, -3.116917426439186123, 8.283357778048666020 ) ) ;
#5402 = CARTESIAN_POINT ( 'NONE',  ( 25.99533317148741318, -3.650983533393564517, -3.627061608673662008 ) ) ;
#5403 = FACE_OUTER_BOUND ( 'NONE', #17841, .T. ) ;
#5404 = ADVANCED_FACE ( 'NONE', ( #9318, #6778 ), #16323, .T. ) ;
#5405 = B_SPLINE_CURVE_WITH_KNOTS ( 'NONE', 3,
 ( #4425, #5949, #13030, #12759 ),
 .UNSPECIFIED., .F., .F.,
 ( 4, 4 ),
 ( 4.336808689942017736E-19, 0.0003446252387907799432 ),
 .UNSPECIFIED. ) ;
#5406 = CARTESIAN_POINT ( 'NONE',  ( 30.03006034954003667, -2.965006068755446478, -3.283357778048662023 ) ) ;
#5407 = CARTESIAN_POINT ( 'NONE',  ( 26.01652455409633902, -4.902371455920926380, -5.783357778048663356 ) ) ;
#5408 = VECTOR ( 'NONE', #306, 1000.000000000000114 ) ;
#5409 = CARTESIAN_POINT ( 'NONE',  ( 29.25000000000000000, -16.21813761408365195, -13.37255996287876236 ) ) ;
#5410 = DIRECTION ( 'NONE',  ( 0.9928203230275511881, 0.1196152422706614482, 0.000000000000000000 ) ) ;
#5411 =( NAMED_UNIT ( * ) PLANE_ANGLE_UNIT ( ) SI_UNIT ( $, .RADIAN. ) );
#5412 = ORIENTED_EDGE ( 'NONE', *, *, #9850, .T. ) ;
#5413 = EDGE_CURVE ( 'NONE', #4427, #9967, #16572, .T. ) ;
#5414 = CARTESIAN_POINT ( 'NONE',  ( 32.30426898124760982, -6.025734024055190652, -6.861505862736167138 ) ) ;
#5415 = CARTESIAN_POINT ( 'NONE',  ( 28.54354359905709160, -7.105797696961086096, -5.783357778048669573 ) ) ;
#5416 = ORIENTED_EDGE ( 'NONE', *, *, #2049, .T. ) ;
#5417 = CARTESIAN_POINT ( 'NONE',  ( -23.00000000000000000, -16.21813761408365195, -13.00000000000000178 ) ) ;
#5418 = CARTESIAN_POINT ( 'NONE',  ( 31.87265695910486230, -5.650636735497883478, -8.283357778048664244 ) ) ;
#5419 = ORIENTED_EDGE ( 'NONE', *, *, #1311, .F. ) ;
#5420 = AXIS2_PLACEMENT_3D ( 'NONE', #14449, #17089, #1759 ) ;
#5421 = EDGE_CURVE ( 'NONE', #2657, #8339, #3526, .T. ) ;
#5422 = VERTEX_POINT ( 'NONE', #16229 ) ;
#5423 = CARTESIAN_POINT ( 'NONE',  ( 31.27962407439061110, -2.387360303286481855, 4.705209693361167567 ) ) ;
#5424 = CARTESIAN_POINT ( 'NONE',  ( 27.12505156253147831, -7.276697974355292864, -5.783357778048668685 ) ) ;
#5425 = DIRECTION ( 'NONE',  ( -0.8660254037844378194, 0.5000000000000014433, 0.000000000000000000 ) ) ;
#5426 = LINE ( 'NONE', #10943, #16252 ) ;
#5427 = CARTESIAN_POINT ( 'NONE',  ( 28.36401332423200827, -6.500457016816879374, -6.861505862736166250 ) ) ;
#5428 = CARTESIAN_POINT ( 'NONE',  ( 26.31556265977298992, -7.384422263489805793, -5.783357778048663356 ) ) ;
#5429 = CARTESIAN_POINT ( 'NONE',  ( 1.243649364574536075E-15, 4.862606272033089816, -3.445885042887437244 ) ) ;
#5430 = FACE_OUTER_BOUND ( 'NONE', #10125, .T. ) ;
#5431 = CARTESIAN_POINT ( 'NONE',  ( 27.84978555093622177, -3.227686124957687586, -8.283357778048658915 ) ) ;
#5432 = COLOUR_RGB ( '', 0.66274510, 0.83137255, 0.94901961) ;
#5433 = VERTEX_POINT ( 'NONE', #9401 ) ;
#5434 = EDGE_CURVE ( 'NONE', #3640, #6169, #4010, .T. ) ;
#5435 = DIRECTION ( 'NONE',  ( 0.000000000000000000, 0.000000000000000000, -1.000000000000000000 ) ) ;
#5436 = AXIS2_PLACEMENT_3D ( 'NONE', #12341, #11049, #17906 ) ;
#5437 = PRESENTATION_STYLE_ASSIGNMENT (( #5344 ) ) ;
#5438 = CARTESIAN_POINT ( 'NONE',  ( 7.374038404635931521, -5.989453865500120600, -2.000000000000000000 ) ) ;
#5439 = CARTESIAN_POINT ( 'NONE',  ( 25.95642634701329499, -4.403549397486640871, -3.686412874245495797 ) ) ;
#5440 = DIRECTION ( 'NONE',  ( -1.000000000000000000, -0.000000000000000000, -0.000000000000000000 ) ) ;
#5441 = CARTESIAN_POINT ( 'NONE',  ( 28.14933959732260149, -3.391468297350500372, -7.939653947423660263 ) ) ;
#5442 = VECTOR ( 'NONE', #12694, 1000.000000000000000 ) ;
#5443 = EDGE_CURVE ( 'NONE', #8628, #11479, #10917, .T. ) ;
#5444 = CARTESIAN_POINT ( 'NONE',  ( 0.000000000000000000, 0.000000000000000000, -10.00000000000000000 ) ) ;
#5445 = VERTEX_POINT ( 'NONE', #2786 ) ;
#5446 = CARTESIAN_POINT ( 'NONE',  ( -3.333333333333332149, -2.694301256218260665, -3.000726591567082657 ) ) ;
#5447 = ORIENTED_EDGE ( 'NONE', *, *, #9395, .F. ) ;
#5448 = CARTESIAN_POINT ( 'NONE',  ( 30.28142597461332741, -2.507623461452779701, -4.705209693361160461 ) ) ;
#5449 = FACE_BOUND ( 'NONE', #17127, .T. ) ;
#5450 = ORIENTED_EDGE ( 'NONE', *, *, #11344, .F. ) ;
#5451 = EDGE_CURVE ( 'NONE', #1012, #4376, #14943, .T. ) ;
#5452 = CARTESIAN_POINT ( 'NONE',  ( 32.54050588463559990, -2.235448945602741766, -6.861505862736159145 ) ) ;
#5453 = EDGE_CURVE ( 'NONE', #11482, #9288, #6447, .T. ) ;
#5454 = CARTESIAN_POINT ( 'NONE',  ( 21.42601376483257880, 2.765314980223224417, 12.00000000000000000 ) ) ;
#5455 = CARTESIAN_POINT ( 'NONE',  ( 31.71807556108801407, -1.697368162559112825, 6.453230759126469707 ) ) ;
#5456 = CARTESIAN_POINT ( 'NONE',  ( 27.02414796481377124, -2.900061135469103490, -6.861505862736158257 ) ) ;
#5457 = AXIS2_PLACEMENT_3D ( 'NONE', #9421, #8920, #4653 ) ;
#5458 = CARTESIAN_POINT ( 'NONE',  ( 29.08935247050201767, -2.014077381790315702, -5.783357778048658027 ) ) ;
#5459 = CIRCLE ( 'NONE', #17084, 2.749999999999995559 ) ;
#5460 = CARTESIAN_POINT ( 'NONE',  ( 28.08810621022444920, -4.652786776866828511, 7.939653947423662039 ) ) ;
#5461 = CARTESIAN_POINT ( 'NONE',  ( -4.197393957002304887, -7.639915766855272736E-14, -3.203767560748932208 ) ) ;
#5462 = ORIENTED_EDGE ( 'NONE', *, *, #9447, .T. ) ;
#5463 = CARTESIAN_POINT ( 'NONE',  ( 31.00199007654869732, -2.847907730748336697, 3.283357778048666464 ) ) ;
#5464 = ORIENTED_EDGE ( 'NONE', *, *, #12835, .T. ) ;
#5465 = AXIS2_PLACEMENT_3D ( 'NONE', #539, #6521, #10658 ) ;
#5466 = CARTESIAN_POINT ( 'NONE',  ( 0.000000000000000000, 0.000000000000000000, -3.000000000000002665 ) ) ;
#5467 = ORIENTED_EDGE ( 'NONE', *, *, #15948, .T. ) ;
#5468 = CARTESIAN_POINT ( 'NONE',  ( -10.27627944162877505, 4.200961894323461010, -11.72793873352925331 ) ) ;
#5469 = B_SPLINE_CURVE_WITH_KNOTS ( 'NONE', 3,
 ( #7553, #7649, #12899, #302, #11332, #483 ),
 .UNSPECIFIED., .F., .F.,
 ( 4, 2, 4 ),
 ( 0.002365888236227979037, 0.003551327329835078910, 0.004736766423442178783 ),
 .UNSPECIFIED. ) ;
#5470 = CARTESIAN_POINT ( 'NONE',  ( 30.82871344409320713, -3.068656662272551738, -7.939653947423660263 ) ) ;
#5471 = FACE_OUTER_BOUND ( 'NONE', #14129, .T. ) ;
#5472 = DIRECTION ( 'NONE',  ( -1.000000000000000000, 0.000000000000000000, 0.000000000000000000 ) ) ;
#5473 = DIRECTION ( 'NONE',  ( -1.000000000000000000, 0.000000000000000000, 0.000000000000000000 ) ) ;
#5474 = CARTESIAN_POINT ( 'NONE',  ( 25.58373587974369201, -2.446631813008643075, 5.783357778048668685 ) ) ;
#5475 = VECTOR ( 'NONE', #13654, 1000.000000000000227 ) ;
#5476 = CARTESIAN_POINT ( 'NONE',  ( 28.56093688906631911, -4.595820017735426255, 7.939653947423662039 ) ) ;
#5477 = EDGE_CURVE ( 'NONE', #17078, #16901, #8353, .T. ) ;
#5478 = DIRECTION ( 'NONE',  ( 1.000000000000000000, 0.000000000000000000, 0.000000000000000000 ) ) ;
#5479 = CARTESIAN_POINT ( 'NONE',  ( -21.42601376483257880, 2.765314980223223529, 0.000000000000000000 ) ) ;
#5480 = CARTESIAN_POINT ( 'NONE',  ( 33.13163345120441505, -4.045141346131868154, 7.939653947423662039 ) ) ;
#5481 = AXIS2_PLACEMENT_3D ( 'NONE', #4657, #12637, #9993 ) ;
#5482 = ORIENTED_EDGE ( 'NONE', *, *, #7086, .T. ) ;
#5483 = EDGE_CURVE ( 'NONE', #5547, #1659, #5669, .T. ) ;
#5484 = VERTEX_POINT ( 'NONE', #12482 ) ;
#5485 = CARTESIAN_POINT ( 'NONE',  ( 32.04158527077989760, -6.057382223572642665, 6.861505862736158257 ) ) ;
#5486 = CARTESIAN_POINT ( 'NONE',  ( 23.00000000000000000, -16.21813761408365195, -13.00000000000000178 ) ) ;
#5487 = EDGE_LOOP ( 'NONE', ( #4654, #17307, #14687, #14006 ) ) ;
#5488 = CARTESIAN_POINT ( 'NONE',  ( 27.23882169172318513, -6.009049854935478052, 3.627061608673662896 ) ) ;
#5489 = CARTESIAN_POINT ( 'NONE',  ( 30.98067518586950442, -1.786210345264705790, -5.783357778048658027 ) ) ;
#5490 = CARTESIAN_POINT ( 'NONE',  ( 27.26436163736424945, -2.571311352887278190, 4.533357778048667797 ) ) ;
#5491 = DIRECTION ( 'NONE',  ( 0.000000000000000000, 0.000000000000000000, 1.000000000000000000 ) ) ;
#5492 = CARTESIAN_POINT ( 'NONE',  ( 27.02414796481377124, -2.900061135469103490, -6.861505862736158257 ) ) ;
#5493 = LINE ( 'NONE', #11014, #17451 ) ;
#5494 = AXIS2_PLACEMENT_3D ( 'NONE', #9954, #1552, #1364 ) ;
#5495 = CARTESIAN_POINT ( 'NONE',  ( 29.98885399772409954, -6.604504582617394703, -4.533357778048668685 ) ) ;
#5496 = FACE_OUTER_BOUND ( 'NONE', #36, .T. ) ;
#5497 = CARTESIAN_POINT ( 'NONE',  ( -4.281152949374479100, 4.203775615332273397, -1.901951201008075243 ) ) ;
#5498 = PLANE ( 'NONE',  #9074 ) ;
#5499 = VERTEX_POINT ( 'NONE', #4238 ) ;
#5500 = EDGE_CURVE ( 'NONE', #13220, #8853, #13564, .T. ) ;
#5501 = CARTESIAN_POINT ( 'NONE',  ( 28.08810621022444920, -4.652786776866828511, -3.627061608673664672 ) ) ;
#5502 = AXIS2_PLACEMENT_3D ( 'NONE', #9526, #6908, #1115 ) ;
#5503 = CARTESIAN_POINT ( 'NONE',  ( 28.51709679197738723, -3.347160818026084339, -3.627061608673662008 ) ) ;
#5504 = AXIS2_PLACEMENT_3D ( 'NONE', #16220, #9049, #11845 ) ;
#5505 = FACE_OUTER_BOUND ( 'NONE', #12742, .T. ) ;
#5506 = FACE_OUTER_BOUND ( 'NONE', #10442, .T. ) ;
#5507 = ORIENTED_EDGE ( 'NONE', *, *, #8777, .T. ) ;
#5508 = ADVANCED_FACE ( 'NONE', ( #7235 ), #12576, .T. ) ;
#5509 = CIRCLE ( 'NONE', #15663, 9.500000000000001776 ) ;
#5510 = ORIENTED_EDGE ( 'NONE', *, *, #5707, .T. ) ;
#5511 =( GEOMETRIC_REPRESENTATION_CONTEXT ( 3 ) GLOBAL_UNCERTAINTY_ASSIGNED_CONTEXT ( ( #15188 ) ) GLOBAL_UNIT_ASSIGNED_CONTEXT ( ( #14598, #16045, #13128 ) ) REPRESENTATION_CONTEXT ( 'NONE', 'WORKASPACE' ) );
#5512 = CARTESIAN_POINT ( 'NONE',  ( 31.93198502805756789, -2.935734224299280548, 3.627061608673666449 ) ) ;
#5513 = CARTESIAN_POINT ( 'NONE',  ( 29.82181869931131146, -4.443908660051686610, -3.627061608673664672 ) ) ;
#5514 = DIRECTION ( 'NONE',  ( -0.1196152422706597551, 0.9928203230275514102, 0.000000000000000000 ) ) ;
#5515 = CARTESIAN_POINT ( 'NONE',  ( 4.000000000000000000, 2.309401076758498483, -4.700000000000000178 ) ) ;
#5516 = LINE ( 'NONE', #6886, #8149 ) ;
#5518 = VECTOR ( 'NONE', #8991, 1000.000000000000000 ) ;
#5517 = CARTESIAN_POINT ( 'NONE',  ( 27.51889869220010354, -3.467423976192371082, -7.939653947423660263 ) ) ;
#5519 = DIRECTION ( 'NONE',  ( 0.9928203230275511881, 0.1196152422706614760, 0.000000000000000000 ) ) ;
#5520 = FACE_OUTER_BOUND ( 'NONE', #7894, .T. ) ;
#5521 = CIRCLE ( 'NONE', #7857, 1.000000000000000000 ) ;
#5522 = CARTESIAN_POINT ( 'NONE',  ( 30.07408527595748282, -27.82894256842317660, -13.18310524188698452 ) ) ;
#5523 = CARTESIAN_POINT ( 'NONE',  ( 26.52132749406794687, -1.933925500942234921, -5.783357778048658027 ) ) ;
#5524 = AXIS2_PLACEMENT_3D ( 'NONE', #13048, #10230, #1917 ) ;
#5525 = CARTESIAN_POINT ( 'NONE',  ( 28.98992747081925359, -3.290194058894681639, -3.627061608673662896 ) ) ;
#5526 = CARTESIAN_POINT ( 'NONE',  ( 28.16881664323204859, -6.096876348486420127, -8.283357778048664244 ) ) ;
#5527 = FACE_OUTER_BOUND ( 'NONE', #14208, .T. ) ;
#5528 = CARTESIAN_POINT ( 'NONE',  ( 20.00000000000000000, 7.999999999999996447, 15.51150668642334374 ) ) ;
#5529 = CARTESIAN_POINT ( 'NONE',  ( 27.71165237056504793, -5.952083095804076684, -7.939653947423662927 ) ) ;
#5530 = VECTOR ( 'NONE', #8071, 1000.000000000000000 ) ;
#5531 = EDGE_LOOP ( 'NONE', ( #15489, #14823 ) ) ;
#5532 = CARTESIAN_POINT ( 'NONE',  ( 39.16489837658902928, -5.353591089051432661, -9.283357778048653586 ) ) ;
#5533 = FACE_OUTER_BOUND ( 'NONE', #2016, .T. ) ;
#5534 = EDGE_CURVE ( 'NONE', #11901, #9058, #1618, .T. ) ;
#5535 = CARTESIAN_POINT ( 'NONE',  ( -18.31874363337315970, -12.05639433133630511, -15.79760360980902689 ) ) ;
#5536 = ORIENTED_EDGE ( 'NONE', *, *, #4293, .F. ) ;
#5537 = CARTESIAN_POINT ( 'NONE',  ( 29.67743187657054449, -6.342216019229654833, -4.705209693361169343 ) ) ;
#5538 = DIRECTION ( 'NONE',  ( 1.224646799147353207E-16, -1.000000000000000000, 0.000000000000000000 ) ) ;
#5539 = CIRCLE ( 'NONE', #17468, 0.9000000000000011324 ) ;
#5540 = CARTESIAN_POINT ( 'NONE',  ( 26.10855331130634127, -2.710563430764044490, -4.533357778048659803 ) ) ;
#5541 = CARTESIAN_POINT ( 'NONE',  ( 29.16815758536418102, -2.004582921727632971, 5.783357778048662468 ) ) ;
#5542 = CYLINDRICAL_SURFACE ( 'NONE', #3115, 2.500000000000001776 ) ;
#5543 = AXIS2_PLACEMENT_3D ( 'NONE', #1414, #10999, #9646 ) ;
#5544 = CARTESIAN_POINT ( 'NONE',  ( 26.60838078660069428, -6.085005533777348319, -7.939653947423664704 ) ) ;
#5545 = AXIS2_PLACEMENT_3D ( 'NONE', #9408, #9660, #2792 ) ;
#5546 = CARTESIAN_POINT ( 'NONE',  ( 17.71310509092289465, -19.55788671310905613, -15.89250038334901305 ) ) ;
#5547 = VERTEX_POINT ( 'NONE', #5581 ) ;
#5548 = CIRCLE ( 'NONE', #16325, 2.500000000000001776 ) ;
#5549 = ADVANCED_FACE ( 'NONE', ( #9737 ), #3061, .T. ) ;
#5550 = DIRECTION ( 'NONE',  ( 0.000000000000000000, 0.000000000000000000, 1.000000000000000000 ) ) ;
#5551 = DIRECTION ( 'NONE',  ( 0.05980762113533058533, -0.4964101615137755386, -0.8660254037844385966 ) ) ;
#5552 = CARTESIAN_POINT ( 'NONE',  ( 28.76992167940542799, -7.088720471389836852, 5.113484796970857005 ) ) ;
#5553 = ORIENTED_EDGE ( 'NONE', *, *, #11040, .T. ) ;
#5554 = AXIS2_PLACEMENT_3D ( 'NONE', #8563, #16731, #2946 ) ;
#5555 = CARTESIAN_POINT ( 'NONE',  ( 28.53771668024168662, -2.080538600569502794, -5.783357778048658027 ) ) ;
#5556 = ORIENTED_EDGE ( 'NONE', *, *, #12099, .T. ) ;
#5557 = CARTESIAN_POINT ( 'NONE',  ( -45.50000000000000000, -16.03270077640482683, 2.787981825772258837 ) ) ;
#5558 = ORIENTED_EDGE ( 'NONE', *, *, #10949, .F. ) ;
#5559 = ORIENTED_EDGE ( 'NONE', *, *, #2253, .F. ) ;
#5560 = CARTESIAN_POINT ( 'NONE',  ( 33.10345976029034887, -2.594722134608779207, -3.283357778048662023 ) ) ;
#5561 = CARTESIAN_POINT ( 'NONE',  ( 29.76058531221316628, -5.705227139567997874, -7.939653947423664704 ) ) ;
#5562 = ORIENTED_EDGE ( 'NONE', *, *, #12061, .F. ) ;
#5563 = CARTESIAN_POINT ( 'NONE',  ( -4.000000000000000000, -0.3979232138631214610, -1.402686560653121361E-15 ) ) ;
#5564 = DIRECTION ( 'NONE',  ( -0.000000000000000000, -0.000000000000000000, 1.000000000000000000 ) ) ;
#5565 = DIRECTION ( 'NONE',  ( 1.000000000000000000, 0.000000000000000000, 0.000000000000000000 ) ) ;
#5566 = LINE ( 'NONE', #11084, #16772 ) ;
#5567 = CARTESIAN_POINT ( 'NONE',  ( 28.97253418081003673, -5.800171738120336151, 3.627061608673662896 ) ) ;
#5568 = CARTESIAN_POINT ( 'NONE',  ( -23.00000000000000000, -16.21813761408365195, -13.00000000000000178 ) ) ;
#5569 = CARTESIAN_POINT ( 'NONE',  ( 26.01652455409633902, -4.902371455920926380, -5.783357778048663356 ) ) ;
#5570 = CARTESIAN_POINT ( 'NONE',  ( 33.33308377457396432, -5.274811626130743392, 7.939653947423658487 ) ) ;
#5571 = VECTOR ( 'NONE', #15820, 1000.000000000000114 ) ;
#5572 = ORIENTED_EDGE ( 'NONE', *, *, #11835, .F. ) ;
#5573 = EDGE_LOOP ( 'NONE', ( #1007, #12937, #12723, #5393 ) ) ;
#5574 = ADVANCED_FACE ( 'NONE', ( #5759 ), #11274, .F. ) ;
#5575 = CARTESIAN_POINT ( 'NONE',  ( 29.39282811755836633, -5.749534618892433002, 7.939653947423658487 ) ) ;
#5576 = AXIS2_PLACEMENT_3D ( 'NONE', #3712, #14614, #5236 ) ;
#5577 = CARTESIAN_POINT ( 'NONE',  ( 27.53153627355490229, -7.237921456612971483, 6.453230759126462601 ) ) ;
#5578 = ORIENTED_EDGE ( 'NONE', *, *, #12618, .F. ) ;
#5579 = CARTESIAN_POINT ( 'NONE',  ( 26.41562710823574278, -3.600346414165641828, 3.627061608673666449 ) ) ;
#5580 = ORIENTED_EDGE ( 'NONE', *, *, #17011, .F. ) ;
#5581 = CARTESIAN_POINT ( 'NONE',  ( -3.248936832696171617, -15.16081378324841111, 17.00000000000000000 ) ) ;
#5582 = DIRECTION ( 'NONE',  ( 0.9928203230275512992, 0.1196152422706614898, -0.000000000000000000 ) ) ;
#5583 = CARTESIAN_POINT ( 'NONE',  ( 31.68992120585416217, -1.700760206360153015, -5.783357778048664244 ) ) ;
#5584 = CARTESIAN_POINT ( 'NONE',  ( 26.62577407660990758, -3.575027854551694695, -3.627061608673662008 ) ) ;
#5585 = DIRECTION ( 'NONE',  ( 1.000000000000000000, 8.881784197001252323E-16, 0.000000000000000000 ) ) ;
#5586 = CARTESIAN_POINT ( 'NONE',  ( 28.49145532429760053, -1.696564004353941613, -5.783357778048658027 ) ) ;
#5587 = CARTESIAN_POINT ( 'NONE',  ( 32.43181250335191379, -6.310176327312596811, -4.533357778048668685 ) ) ;
#5588 = DIRECTION ( 'NONE',  ( 0.9928203230275512992, 0.1196152422706607682, -0.000000000000000000 ) ) ;
#5589 = CARTESIAN_POINT ( 'NONE',  ( 26.29446227649215473, -10.90310086042137350, 14.16253947949896563 ) ) ;
#5590 = CARTESIAN_POINT ( 'NONE',  ( 29.49337484321020497, -2.602568060005117090, -4.705209693361161349 ) ) ;
#5591 = CARTESIAN_POINT ( 'NONE',  ( 27.67650891848073158, -3.448435056481901295, -7.939653947423660263 ) ) ;
#5592 = EDGE_LOOP ( 'NONE', ( #15951, #15562, #4867, #8977 ) ) ;
#5593 = CARTESIAN_POINT ( 'NONE',  ( 30.03006034954003667, -2.965006068755446478, -3.283357778048662023 ) ) ;
#5594 = AXIS2_PLACEMENT_3D ( 'NONE', #6163, #9789, #14421 ) ;
#5595 = ORIENTED_EDGE ( 'NONE', *, *, #17, .T. ) ;
#5596 = EDGE_LOOP ( 'NONE', ( #16986, #16547 ) ) ;
#5597 = CARTESIAN_POINT ( 'NONE',  ( 27.61527553138257574, -4.709753535998224550, 3.627061608673664228 ) ) ;
#5598 = CARTESIAN_POINT ( 'NONE',  ( 25.95642634701329499, -4.403549397486640871, -3.686412874245495352 ) ) ;
#5599 = PLANE ( 'NONE',  #10349 ) ;
#5600 = EDGE_CURVE ( 'NONE', #14870, #13858, #7057, .T. ) ;
#5601 = CARTESIAN_POINT ( 'NONE',  ( 32.95080301609915097, -1.548848848676412482, -5.783357778048662468 ) ) ;
#5602 = DIRECTION ( 'NONE',  ( 0.9928203230275512992, 0.1196152422706610180, 4.006172263299093133E-17 ) ) ;
#5603 = CARTESIAN_POINT ( 'NONE',  ( 30.02326902268086428, -5.673578940050561847, -3.627061608673667781 ) ) ;
#5604 = CARTESIAN_POINT ( 'NONE',  ( 31.88017671309158274, -6.376637546091784792, -4.533357778048668685 ) ) ;
#5605 = CARTESIAN_POINT ( 'NONE',  ( 37.11592063525292673, -0.6724158536360932414, -10.75768461118259545 ) ) ;
#5606 = CIRCLE ( 'NONE', #7097, 3.000000000000000000 ) ;
#5607 = DIRECTION ( 'NONE',  ( -0.1196152422706610735, 0.9928203230275511881, 0.000000000000000000 ) ) ;
#5608 = CARTESIAN_POINT ( 'NONE',  ( 29.23078034989804763, -4.515117109069654688, -8.283357778048662468 ) ) ;
#5609 = EDGE_CURVE ( 'NONE', #9143, #122, #9836, .T. ) ;
#5610 = ORIENTED_EDGE ( 'NONE', *, *, #378, .T. ) ;
#5611 = CARTESIAN_POINT ( 'NONE',  ( 30.02326902268086428, -5.673578940050561847, -3.627061608673667781 ) ) ;
#5612 = PLANE ( 'NONE',  #3687 ) ;
#5613 = DIRECTION ( 'NONE',  ( 1.000000000000000000, 0.000000000000000000, -0.000000000000000000 ) ) ;
#5614 = CARTESIAN_POINT ( 'NONE',  ( 33.69269431359690969, -6.158264969628857166, 7.033357778048657138 ) ) ;
#5615 = CARTESIAN_POINT ( 'NONE',  ( 28.24571643650507369, -4.633797857156355171, -7.939653947423662039 ) ) ;
#5616 = ORIENTED_EDGE ( 'NONE', *, *, #5183, .F. ) ;
#5617 = ORIENTED_EDGE ( 'NONE', *, *, #2301, .F. ) ;
#5618 = FACE_OUTER_BOUND ( 'NONE', #11965, .T. ) ;
#5619 = CYLINDRICAL_SURFACE ( 'NONE', #17146, 2.000000000000001776 ) ;
#5620 = EDGE_LOOP ( 'NONE', ( #7306, #4544, #7105, #16938 ) ) ;
#5621 = FACE_OUTER_BOUND ( 'NONE', #8937, .T. ) ;
#5622 = ORIENTED_EDGE ( 'NONE', *, *, #10415, .T. ) ;
#5623 = CARTESIAN_POINT ( 'NONE',  ( 28.28502977505876359, -2.748149777785362957, -6.861505862736158257 ) ) ;
#5624 = DIRECTION ( 'NONE',  ( -1.000000000000000000, 0.000000000000000000, 0.000000000000000000 ) ) ;
#5625 = ADVANCED_FACE ( 'NONE', ( #9929 ), #156, .F. ) ;
#5626 = VERTEX_POINT ( 'NONE', #8495 ) ;
#5627 = ORIENTED_EDGE ( 'NONE', *, *, #11024, .T. ) ;
#5628 = CARTESIAN_POINT ( 'NONE',  ( 30.64918316926811315, -2.463315982128351678, -6.861505862736159145 ) ) ;
#5629 = DIRECTION ( 'NONE',  ( -0.000000000000000000, -0.000000000000000000, 1.000000000000000000 ) ) ;
#5630 = CARTESIAN_POINT ( 'NONE',  ( 4.000000000000000000, 0.8378468363844291389, -2.920592527564379370 ) ) ;
#5631 = ORIENTED_EDGE ( 'NONE', *, *, #1305, .T. ) ;
#5632 = CARTESIAN_POINT ( 'NONE',  ( 30.30397292480292037, -1.478191427891014431, -5.783357778048658027 ) ) ;
#5633 = ADVANCED_FACE ( 'NONE', ( #15478 ), #17233, .F. ) ;
#5634 = EDGE_LOOP ( 'NONE', ( #4471, #213, #9562, #9242 ) ) ;
#5635 = CARTESIAN_POINT ( 'NONE',  ( 30.00264913441657555, -6.940201157507134511, -5.783357778048657138 ) ) ;
#5636 = ORIENTED_EDGE ( 'NONE', *, *, #6443, .F. ) ;
#5637 = CARTESIAN_POINT ( 'NONE',  ( 26.78782184427022983, -4.809445364374452581, 3.283357778048664244 ) ) ;
#5638 = AXIS2_PLACEMENT_3D ( 'NONE', #16305, #5299, #8031 ) ;
#5639 = SHAPE_REPRESENTATION ( 'Caliper Body Half', ( #3575 ), #2991 ) ;
#5640 = ADVANCED_FACE ( 'NONE', ( #11840 ), #6230, .F. ) ;
#5641 = DIRECTION ( 'NONE',  ( -1.224646799147353207E-16, 1.000000000000000000, 0.000000000000000000 ) ) ;
#5642 = SURFACE_STYLE_USAGE ( .BOTH. , #16725 ) ;
#5643 = LINE ( 'NONE', #8651, #15902 ) ;
#5644 = ORIENTED_EDGE ( 'NONE', *, *, #6436, .F. ) ;
#5645 = CARTESIAN_POINT ( 'NONE',  ( 31.29168529989541270, -6.784897756022354010, 5.113484796970852564 ) ) ;
#5646 = ORIENTED_EDGE ( 'NONE', *, *, #15211, .T. ) ;
#5647 = CARTESIAN_POINT ( 'NONE',  ( 26.61823960964035507, -2.311797680896151341, 5.113484796970861446 ) ) ;
#5648 = ORIENTED_EDGE ( 'NONE', *, *, #8958, .F. ) ;
#5649 = DIRECTION ( 'NONE',  ( 1.000000000000000000, 0.000000000000000000, 0.000000000000000000 ) ) ;
#5650 = CARTESIAN_POINT ( 'NONE',  ( 26.39370705969127684, -2.976016814310973313, -6.861505862736158257 ) ) ;
#5651 = CYLINDRICAL_SURFACE ( 'NONE', #4588, 2.500000000000001776 ) ;
#5652 = CARTESIAN_POINT ( 'NONE',  ( 2.500000000000000000, -1.178949249685213863, 2.042000000000001148 ) ) ;
#5653 = PRODUCT_CONTEXT ( 'NONE', #14562, 'mechanical' ) ;
#5654 = CYLINDRICAL_SURFACE ( 'NONE', #12999, 6.000000000000000888 ) ;
#5655 = CARTESIAN_POINT ( 'NONE',  ( 29.51982165028991645, -6.361204938940122844, 6.861505862736158257 ) ) ;
#5656 = EDGE_CURVE ( 'NONE', #6446, #17327, #5122, .T. ) ;
#5657 = LINE ( 'NONE', #5841, #14269 ) ;
#5658 = DIRECTION ( 'NONE',  ( -0.1196152422706610735, 0.9928203230275511881, 0.000000000000000000 ) ) ;
#5659 = CARTESIAN_POINT ( 'NONE',  ( 29.66420847303068697, -4.462897579762144851, 3.627061608673664228 ) ) ;
#5660 = ORIENTED_EDGE ( 'NONE', *, *, #8666, .F. ) ;
#5661 = ORIENTED_EDGE ( 'NONE', *, *, #201, .F. ) ;
#5662 = CARTESIAN_POINT ( 'NONE',  ( 26.98483462626008134, -4.785709214840094816, 3.627061608673664228 ) ) ;
#5663 = CARTESIAN_POINT ( 'NONE',  ( 31.74131510559286085, -5.666460835049167422, -3.283357778048667797 ) ) ;
#5664 = CARTESIAN_POINT ( 'NONE',  ( 23.00000000000000000, -16.21813761408365195, 13.00000000000000178 ) ) ;
#5665 = ADVANCED_FACE ( 'NONE', ( #9304 ), #17519, .F. ) ;
#5666 = VERTEX_POINT ( 'NONE', #14493 ) ;
#5667 = CARTESIAN_POINT ( 'NONE',  ( 30.72436838703367812, -6.515889623968540434, 4.533357778048659803 ) ) ;
#5668 = ORIENTED_EDGE ( 'NONE', *, *, #4173, .F. ) ;
#5669 = LINE ( 'NONE', #12750, #8063 ) ;
#5670 = CYLINDRICAL_SURFACE ( 'NONE', #10102, 1.000000000000000000 ) ;
#5671 = CARTESIAN_POINT ( 'NONE',  ( 32.95080301609915097, -1.548848848676412260, -5.783357778048663356 ) ) ;
#5672 = CARTESIAN_POINT ( 'NONE',  ( 27.91310269393460430, -7.181753375802955475, -5.783357778048669573 ) ) ;
#5673 = CARTESIAN_POINT ( 'NONE',  ( 26.18940839444933033, -6.337336286969802224, -7.823481096485427777 ) ) ;
#5674 = CARTESIAN_POINT ( 'NONE',  ( 30.38277803966508372, -1.468696967828331701, -5.783357778048658027 ) ) ;
#5675 = CARTESIAN_POINT ( 'NONE',  ( 29.24999999999999645, -15.80522841342829921, -13.37255996287877480 ) ) ;
#5676 = CARTESIAN_POINT ( 'NONE',  ( 29.04511322243489602, -14.57839366656647506, 13.43065377816253481 ) ) ;
#5677 = CARTESIAN_POINT ( 'NONE',  ( 31.08270050955629671, -4.291997302367946077, -3.627061608673664672 ) ) ;
#5678 = ORIENTED_EDGE ( 'NONE', *, *, #7938, .F. ) ;
#5679 = EDGE_CURVE ( 'NONE', #7873, #1701, #2078, .T. ) ;
#5680 = DIRECTION ( 'NONE',  ( -0.1196152422706621143, 0.9928203230275509661, 0.000000000000000000 ) ) ;
#5681 = CARTESIAN_POINT ( 'NONE',  ( 0.000000000000000000, 0.000000000000000000, -2.000000000000000000 ) ) ;
#5682 = EDGE_LOOP ( 'NONE', ( #15754, #13604, #16656, #1907 ) ) ;
#5683 = ORIENTED_EDGE ( 'NONE', *, *, #17475, .F. ) ;
#5684 = ORIENTED_EDGE ( 'NONE', *, *, #10282, .F. ) ;
#5685 = CARTESIAN_POINT ( 'NONE',  ( 29.62489513447700062, -6.348545659133139729, 4.705209693361160461 ) ) ;
#5686 = CARTESIAN_POINT ( 'NONE',  ( 29.14074637024071990, -5.979778010479330774, -3.283357778048667797 ) ) ;
#5687 = CARTESIAN_POINT ( 'NONE',  ( -25.11802603177690330, -19.03270077640483038, -0.5379818257722508434 ) ) ;
#5688 = VECTOR ( 'NONE', #17756, 1000.000000000000000 ) ;
#5689 = CARTESIAN_POINT ( 'NONE',  ( 25.78902048130849067, -3.014061381488925218, -4.757751673912568258 ) ) ;
#5690 = PLANE ( 'NONE',  #10166 ) ;
#5691 = CARTESIAN_POINT ( 'NONE',  ( 28.86293393808771057, -2.678523738846987357, -4.705209693361161349 ) ) ;
#5692 = CARTESIAN_POINT ( 'NONE',  ( 45.50000000000000000, -19.03270077640483038, -8.287981825772241962 ) ) ;
#5693 = CARTESIAN_POINT ( 'NONE',  ( 26.31556265977298992, -7.384422263489805793, -5.783357778048663356 ) ) ;
#5694 = CARTESIAN_POINT ( 'NONE',  ( 27.30498922523054617, -2.229057914452205136, -5.113484796970851676 ) ) ;
#5695 = CARTESIAN_POINT ( 'NONE',  ( 27.78220930431293922, -1.782014143258494832, -5.783357778048658027 ) ) ;
#5696 = PRODUCT_DEFINITION_FORMATION_WITH_SPECIFIED_SOURCE ( 'ANY', '', #8095, .NOT_KNOWN. ) ;
#5697 = CARTESIAN_POINT ( 'NONE',  ( 30.86385689617752348, -5.572304701594726239, -7.939653947423664704 ) ) ;
#5698 = FACE_OUTER_BOUND ( 'NONE', #7215, .T. ) ;
#5699 = CARTESIAN_POINT ( 'NONE',  ( 0.000000000000000000, 0.000000000000000000, -2.000000000000000000 ) ) ;
#5700 = CARTESIAN_POINT ( 'NONE',  ( 4.197393957002304887, -0.4069871074557454560, -3.203767560748928211 ) ) ;
#5701 = CARTESIAN_POINT ( 'NONE',  ( 46.05330090215556282, 0.2364164235710524975, -5.783357778048662468 ) ) ;
#5702 = EDGE_CURVE ( 'NONE', #9563, #12636, #6031, .T. ) ;
#5703 = AXIS2_PLACEMENT_3D ( 'NONE', #3387, #9008, #11529 ) ;
#5704 = CARTESIAN_POINT ( 'NONE',  ( 31.75254397038802878, -4.211294393702175398, 3.283357778048664244 ) ) ;
#5705 = CARTESIAN_POINT ( 'NONE',  ( 28.97253418081003673, -5.800171738120336151, -7.939653947423662927 ) ) ;
#5706 = ORIENTED_EDGE ( 'NONE', *, *, #8457, .T. ) ;
#5707 = EDGE_CURVE ( 'NONE', #14370, #17637, #10127, .T. ) ;
#5708 = ORIENTED_EDGE ( 'NONE', *, *, #15440, .T. ) ;
#5709 = DIRECTION ( 'NONE',  ( 0.000000000000000000, -0.5000000000000009992, -0.8660254037844380415 ) ) ;
#5710 = DIRECTION ( 'NONE',  ( 0.000000000000000000, 0.000000000000000000, -1.000000000000000000 ) ) ;
#5711 = ADVANCED_BREP_SHAPE_REPRESENTATION ( '', ( #17325, #3575 ), #5366 ) ;
#5712 = ORIENTED_EDGE ( 'NONE', *, *, #2168, .T. ) ;
#5713 = CARTESIAN_POINT ( 'NONE',  ( -20.46503100693326260, -10.50166121531458430, -15.42720773483998009 ) ) ;
#5714 = ORIENTED_EDGE ( 'NONE', *, *, #15901, .F. ) ;
#5715 = CARTESIAN_POINT ( 'NONE',  ( 35.77680296528374271, -19.03270077640483038, -0.5379818257722508434 ) ) ;
#5716 = ORIENTED_EDGE ( 'NONE', *, *, #9764, .T. ) ;
#5717 = CARTESIAN_POINT ( 'NONE',  ( 31.08270050955629671, -4.291997302367946077, -3.627061608673664672 ) ) ;
#5718 = CARTESIAN_POINT ( 'NONE',  ( 0.000000000000000000, 0.000000000000000000, -8.700000000000001066 ) ) ;
#5719 = CARTESIAN_POINT ( 'NONE',  ( 31.92138306490751987, -2.737139032229836566, 8.283357778048666020 ) ) ;
#5720 = CARTESIAN_POINT ( 'NONE',  ( 32.96459815279162342, -1.884545423566157174, -4.533357778048659803 ) ) ;
#5721 = EDGE_CURVE ( 'NONE', #17698, #12650, #3418, .T. ) ;
#5722 = CARTESIAN_POINT ( 'NONE',  ( 31.58296173575813981, -1.713646710223874381, -6.453230759126465266 ) ) ;
#5723 = B_SPLINE_CURVE_WITH_KNOTS ( 'NONE', 3,
 ( #7440, #11684, #3443, #13146, #2005, #7530, #7009, #8973 ),
 .UNSPECIFIED., .F., .F.,
 ( 4, 2, 2, 4 ),
 ( 0.000000000000000000, 0.002450665683189818395, 0.003675998524784727592, 0.004901331366379636789 ),
 .UNSPECIFIED. ) ;
#5724 = CARTESIAN_POINT ( 'NONE',  ( 25.96969170380761582, -2.000386719721422235, 5.783357778048668685 ) ) ;
#5725 =( BOUNDED_CURVE ( )  B_SPLINE_CURVE ( 2, ( #2039, #15905, #11899, #17482, #3660, #9100, #14641, #15729, #5009 ),
 .UNSPECIFIED., .F., .T. ) 
 B_SPLINE_CURVE_WITH_KNOTS ( ( 3, 2, 2, 2, 3 ),
 ( 0.3653846153846154188, 0.3717948717948718063, 0.3846153846153846367, 0.3974358974358974117, 0.4038461538461538547 ),
 .UNSPECIFIED. ) 
 CURVE ( )  GEOMETRIC_REPRESENTATION_ITEM ( )  RATIONAL_B_SPLINE_CURVE ( ( 0.9330127018922194093, 0.9330127018922196314, 1.000000000000000000, 0.8660254037844387076, 1.000000000000000000, 0.8660254037844387076, 1.000000000000000000, 0.9330127018922190762, 0.9330127018922194093 ) ) 
 REPRESENTATION_ITEM ( '' )  );
#5726 = TOROIDAL_SURFACE ( 'NONE', #13566, 12.70000000000000284, 0.9000000000000003553 ) ;
#5727 = ADVANCED_FACE ( 'NONE', ( #14596 ), #2172, .F. ) ;
#5728 = APPLICATION_CONTEXT ( 'automotive_design' ) ;
#5729 = ADVANCED_FACE ( 'NONE', ( #14673 ), #8420, .F. ) ;
#5730 = DIRECTION ( 'NONE',  ( -0.1196152422706624058, 0.9928203230275510771, 0.000000000000000000 ) ) ;
#5731 =( NAMED_UNIT ( * ) PLANE_ANGLE_UNIT ( ) SI_UNIT ( $, .RADIAN. ) );
#5732 = DIRECTION ( 'NONE',  ( 1.000000000000000000, 0.000000000000000000, 0.000000000000000000 ) ) ;
#5733 = ORIENTED_EDGE ( 'NONE', *, *, #17759, .F. ) ;
#5734 = CARTESIAN_POINT ( 'NONE',  ( 28.84872679426759845, -7.079226011327149237, 5.113484796970851676 ) ) ;
#5735 = ORIENTED_EDGE ( 'NONE', *, *, #13760, .T. ) ;
#5736 = LINE ( 'NONE', #16825, #10690 ) ;
#5737 = ORIENTED_EDGE ( 'NONE', *, *, #6008, .F. ) ;
#5738 = DIRECTION ( 'NONE',  ( 0.9928203230275512992, 0.1196152422706610180, 4.006172263299093133E-17 ) ) ;
#5739 = CARTESIAN_POINT ( 'NONE',  ( 27.67650891848073158, -3.448435056481901295, -7.939653947423660263 ) ) ;
#5740 = VECTOR ( 'NONE', #5822, 1000.000000000000227 ) ;
#5741 = CARTESIAN_POINT ( 'NONE',  ( 31.01321894478757812, -1.392741288986461212, -5.783357778048658027 ) ) ;
#5742 = FACE_OUTER_BOUND ( 'NONE', #15981, .T. ) ;
#5743 = PRODUCT_CONTEXT ( 'NONE', #17711, 'mechanical' ) ;
#5744 = CARTESIAN_POINT ( 'NONE',  ( 45.50000000000000000, -16.03270077640482683, 5.537981825772250843 ) ) ;
#5745 = CARTESIAN_POINT ( 'NONE',  ( 5.200000000000002842, 3.061616997868383634E-16, -2.500000000000000444 ) ) ;
#5746 = CARTESIAN_POINT ( 'NONE',  ( 28.08317206381523334, -7.171460237833785278, -5.113484796970862334 ) ) ;
#5747 = CARTESIAN_POINT ( 'NONE',  ( 32.06776442294927421, -4.173316554281249147, 8.283357778048662468 ) ) ;
#5748 = CARTESIAN_POINT ( 'NONE',  ( 30.91186687973582536, -2.431667782610909434, 6.861505862736166250 ) ) ;
#5749 = AXIS2_PLACEMENT_3D ( 'NONE', #17582, #13468, #9450 ) ;
#5750 = ORIENTED_EDGE ( 'NONE', *, *, #11050, .F. ) ;
#5751 = VECTOR ( 'NONE', #2364, 1000.000000000000000 ) ;
#5752 = ORIENTED_EDGE ( 'NONE', *, *, #13314, .T. ) ;
#5753 = CARTESIAN_POINT ( 'NONE',  ( 28.23249303296521617, -2.754479417688857179, 6.861505862736165362 ) ) ;
#5754 = CARTESIAN_POINT ( 'NONE',  ( -4.197393957002304887, -7.639915766855272736E-14, -3.203767560748932208 ) ) ;
#5755 = CARTESIAN_POINT ( 'NONE',  ( 26.03726795043090547, -3.446058701420613879, -8.283357778048660691 ) ) ;
#5756 = ORIENTED_EDGE ( 'NONE', *, *, #16630, .T. ) ;
#5757 = CARTESIAN_POINT ( 'NONE',  ( 28.41655006632555569, -6.494127376913395366, 6.861505862736157368 ) ) ;
#5758 = ORIENTED_EDGE ( 'NONE', *, *, #17205, .T. ) ;
#5759 = FACE_OUTER_BOUND ( 'NONE', #13693, .T. ) ;
#5760 = CARTESIAN_POINT ( 'NONE',  ( 38.37070961486131182, 1.238267339652773913, -5.783357778048661579 ) ) ;
#5761 = EDGE_CURVE ( 'NONE', #12543, #364, #8438, .T. ) ;
#5762 = CARTESIAN_POINT ( 'NONE',  ( 33.95908713831676096, -3.945449517755638791, -3.283357778048664688 ) ) ;
#5763 = CARTESIAN_POINT ( 'NONE',  ( -10.47816170930907553, 0.6768509389586230274, -6.005572809000082835 ) ) ;
#5764 = CIRCLE ( 'NONE', #15923, 3.999999999999998224 ) ;
#5765 = CARTESIAN_POINT ( 'NONE',  ( 32.50309786422735669, -5.574681056656013212, -8.283357778048664244 ) ) ;
#5766 = CARTESIAN_POINT ( 'NONE',  ( 30.25524682244395436, -4.391689130744175884, -3.283357778048664688 ) ) ;
#5767 = CYLINDRICAL_SURFACE ( 'NONE', #3461, 5.500000000000000888 ) ;
#5768 = DIRECTION ( 'NONE',  ( -0.000000000000000000, 1.000000000000000000, -3.469446951953614189E-16 ) ) ;
#5769 = PRODUCT_CONTEXT ( 'NONE', #17836, 'mechanical' ) ;
#5770 = CARTESIAN_POINT ( 'NONE',  ( 31.41114436565740320, -6.133337902414513820, -4.705209693361168455 ) ) ;
#5771 = ORIENTED_EDGE ( 'NONE', *, *, #3022, .T. ) ;
#5772 = AXIS2_PLACEMENT_3D ( 'NONE', #16877, #9950, #4610 ) ;
#5773 = ADVANCED_FACE ( 'NONE', ( #16552 ), #15596, .T. ) ;
#5774 = PLANE ( 'NONE',  #11884 ) ;
#5775 = ORIENTED_EDGE ( 'NONE', *, *, #11616, .T. ) ;
#5776 = VECTOR ( 'NONE', #12916, 1000.000000000000114 ) ;
#5777 = ORIENTED_EDGE ( 'NONE', *, *, #4365, .F. ) ;
#5778 = ORIENTED_EDGE ( 'NONE', *, *, #5296, .T. ) ;
#5779 = CARTESIAN_POINT ( 'NONE',  ( 27.30005507882132676, -4.747731375419166788, 7.939653947423662039 ) ) ;
#5780 = CARTESIAN_POINT ( 'NONE',  ( 32.83754810739939956, -9.116730809865838836, 5.783357778048664244 ) ) ;
#5781 = DIRECTION ( 'NONE',  ( 0.9396926207859104263, 0.000000000000000000, 0.3420201433256631618 ) ) ;
#5782 = CIRCLE ( 'NONE', #10120, 11.80000000000000249 ) ;
#5783 = FACE_OUTER_BOUND ( 'NONE', #14169, .T. ) ;
#5784 = ADVANCED_FACE ( 'NONE', ( #52 ), #11082, .T. ) ;
#5785 = CARTESIAN_POINT ( 'NONE',  ( 29.42285898892238549, -7.010054420087358018, -5.113484796970856117 ) ) ;
#5786 = CARTESIAN_POINT ( 'NONE',  ( 29.38830135902312080, -2.615227339812091767, -6.861505862736159145 ) ) ;
#5787 = CARTESIAN_POINT ( 'NONE',  ( 29.19631194059803292, -2.001190877926593004, -5.113484796970855228 ) ) ;
#5788 = ADVANCED_FACE ( 'NONE', ( #8380, #8029 ), #9466, .T. ) ;
#5789 = CARTESIAN_POINT ( 'NONE',  ( 26.31556265977298992, -7.384422263489805793, -5.783357778048663356 ) ) ;
#5790 = EDGE_LOOP ( 'NONE', ( #12749, #12183, #14356, #11226 ) ) ;
#5791 = FACE_OUTER_BOUND ( 'NONE', #439, .T. ) ;
#5792 = VECTOR ( 'NONE', #2419, 1000.000000000000000 ) ;
#5793 = CARTESIAN_POINT ( 'NONE',  ( -4.914599809708808387, 17.56967244544484075, 17.00000000000000711 ) ) ;
#5794 = ORIENTED_EDGE ( 'NONE', *, *, #13749, .T. ) ;
#5795 = CARTESIAN_POINT ( 'NONE',  ( 30.27725608814395031, -6.896919580145944195, -5.783357778048668685 ) ) ;
#5796 = CARTESIAN_POINT ( 'NONE',  ( 31.24973580796908834, -6.452593224933654170, -4.533357778048668685 ) ) ;
#5797 = LINE ( 'NONE', #4093, #4543 ) ;
#5798 = CARTESIAN_POINT ( 'NONE',  ( 26.31308423962587995, -7.363851090081254824, -5.799730202602000340 ) ) ;
#5799 = CARTESIAN_POINT ( 'NONE',  ( 33.32864623319426300, -4.021405196597508613, 8.283357778048662468 ) ) ;
#5800 = CARTESIAN_POINT ( 'NONE',  ( 27.08121146544255353, -6.028038774645947839, -7.939653947423662927 ) ) ;
#5801 = ORIENTED_EDGE ( 'NONE', *, *, #3088, .F. ) ;
#5802 = CIRCLE ( 'NONE', #12188, 12.50000000000000000 ) ;
#5803 = LINE ( 'NONE', #13985, #6748 ) ;
#5804 = DIRECTION ( 'NONE',  ( 1.000000000000000000, 0.000000000000000000, 0.000000000000000000 ) ) ;
#5805 = ORIENTED_EDGE ( 'NONE', *, *, #5156, .F. ) ;
#5806 = CARTESIAN_POINT ( 'NONE',  ( -18.90926271784950075, -11.47470670281267857, -15.70082023719634989 ) ) ;
#5807 = ORIENTED_EDGE ( 'NONE', *, *, #11555, .F. ) ;
#5808 = AXIS2_PLACEMENT_3D ( 'NONE', #1828, #12959, #542 ) ;
#5809 = CARTESIAN_POINT ( 'NONE',  ( 28.49970350196817392, -5.857138497251737519, -7.939653947423662927 ) ) ;
#5810 = CARTESIAN_POINT ( 'NONE',  ( 30.67110321781257909, -3.087645581983020637, -7.939653947423660263 ) ) ;
#5811 = AXIS2_PLACEMENT_3D ( 'NONE', #8049, #16231, #17537 ) ;
#5812 = ADVANCED_FACE ( 'NONE', ( #2683 ), #1059, .T. ) ;
#5813 = CARTESIAN_POINT ( 'NONE',  ( 30.05329989404488700, -6.934098741245490416, 6.453230759126467042 ) ) ;
#5814 = FACE_BOUND ( 'NONE', #10746, .T. ) ;
#5815 = CARTESIAN_POINT ( 'NONE',  ( 31.17093069310692499, -6.462087684996337345, -4.533357778048668685 ) ) ;
#5816 = CARTESIAN_POINT ( 'NONE',  ( 31.90644508241650357, -6.373472726347483963, -7.033357778048666908 ) ) ;
#5817 = ORIENTED_EDGE ( 'NONE', *, *, #16914, .F. ) ;
#5818 = CARTESIAN_POINT ( 'NONE',  ( 26.27749392786457250, -6.324743385012029151, 3.283357778048663800 ) ) ;
#5819 = AXIS2_PLACEMENT_3D ( 'NONE', #12795, #7280, #4369 ) ;
#5820 = CARTESIAN_POINT ( 'NONE',  ( 39.99999999999999289, 0.000000000000000000, 0.000000000000000000 ) ) ;
#5821 = CARTESIAN_POINT ( 'NONE',  ( -29.25000000000000000, -16.21813761408365195, 13.37255996287876947 ) ) ;
#5822 = DIRECTION ( 'NONE',  ( 0.9928203230275510771, 0.1196152422706614621, -0.000000000000000000 ) ) ;
#5823 = VECTOR ( 'NONE', #1786, 1000.000000000000000 ) ;
#5824 = ORIENTED_EDGE ( 'NONE', *, *, #6253, .T. ) ;
#5825 = CARTESIAN_POINT ( 'NONE',  ( 28.11132641904908169, -7.168068194032743534, -5.783357778048668685 ) ) ;
#5826 = ORIENTED_EDGE ( 'NONE', *, *, #5828, .F. ) ;
#5827 = DIRECTION ( 'NONE',  ( -0.000000000000000000, -1.000000000000000000, 0.000000000000000000 ) ) ;
#5828 = EDGE_CURVE ( 'NONE', #8562, #2496, #13261, .T. ) ;
#5829 = ORIENTED_EDGE ( 'NONE', *, *, #756, .T. ) ;
#5830 = CARTESIAN_POINT ( 'NONE',  ( 33.95908713831673964, -3.945449517755637014, 5.783357778048663356 ) ) ;
#5831 = CARTESIAN_POINT ( 'NONE',  ( 26.52522735095806894, -6.721994413439005278, -4.705209693361169343 ) ) ;
#5832 = CIRCLE ( 'NONE', #8171, 12.50000000000000000 ) ;
#5833 = CARTESIAN_POINT ( 'NONE',  ( 32.01903832059031174, -7.086814257134402162, -5.783357778048669573 ) ) ;
#5834 = CARTESIAN_POINT ( 'NONE',  ( -4.000000000000000000, 0.7924765000094609046, -0.05906175389889908173 ) ) ;
#5835 = PRODUCT_CONTEXT ( 'NONE', #13620, 'mechanical' ) ;
#5836 = CARTESIAN_POINT ( 'NONE',  ( 30.80688261270428541, -4.325227911964988792, -3.283357778048664688 ) ) ;
#5837 = EDGE_CURVE ( 'NONE', #2657, #9429, #16467, .T. ) ;
#5838 =( BOUNDED_CURVE ( )  B_SPLINE_CURVE ( 2, ( #2223, #17573, #6376, #844, #10444, #6478, #17382, #3478, #7738 ),
 .UNSPECIFIED., .F., .T. ) 
 B_SPLINE_CURVE_WITH_KNOTS ( ( 3, 2, 2, 2, 3 ),
 ( 0.7884615384615384359, 0.7948717948717948234, 0.8076923076923077094, 0.8205128205128204844, 0.8269230769230769829 ),
 .UNSPECIFIED. ) 
 CURVE ( )  GEOMETRIC_REPRESENTATION_ITEM ( )  RATIONAL_B_SPLINE_CURVE ( ( 0.9330127018922194093, 0.9330127018922194093, 1.000000000000000000, 0.8660254037844387076, 1.000000000000000000, 0.8660254037844387076, 1.000000000000000000, 0.9330127018922187432, 0.9330127018922192983 ) ) 
 REPRESENTATION_ITEM ( '' )  );
#5839 = CARTESIAN_POINT ( 'NONE',  ( 29.34898802046944155, -4.500875419183088866, -3.627061608673664672 ) ) ;
#5840 = CARTESIAN_POINT ( 'NONE',  ( -2.016448651773435938E-27, -20.49999999999999645, -13.00000000000000178 ) ) ;
#5841 = CARTESIAN_POINT ( 'NONE',  ( 25.74999999999999289, -16.21813761408365195, 13.00000000000000178 ) ) ;
#5842 = CARTESIAN_POINT ( 'NONE',  ( 32.52441275490655670, -6.636378442139655220, 5.783357778048664244 ) ) ;
#5843 = CARTESIAN_POINT ( 'NONE',  ( 31.45915434921569798, -2.992700983430681028, 3.627061608673666893 ) ) ;
#5844 = EDGE_LOOP ( 'NONE', ( #3075, #17873, #7658, #5075 ) ) ;
#5845 = CIRCLE ( 'NONE', #3553, 2.705189185291143605 ) ;
#5846 = AXIS2_PLACEMENT_3D ( 'NONE', #15033, #15210, #4164 ) ;
#5847 = ORIENTED_EDGE ( 'NONE', *, *, #9787, .F. ) ;
#5848 = CARTESIAN_POINT ( 'NONE',  ( 27.73357241910951743, -6.576412695658750529, 4.705209693361160461 ) ) ;
#5849 = SURFACE_SIDE_STYLE ('',( #16747 ) ) ;
#5850 = FACE_OUTER_BOUND ( 'NONE', #6893, .T. ) ;
#5851 = ORIENTED_EDGE ( 'NONE', *, *, #7285, .F. ) ;
#5852 = SURFACE_STYLE_FILL_AREA ( #345 ) ;
#5853 = CARTESIAN_POINT ( 'NONE',  ( -4.000000000000000000, 2.471529427528105227, -3.386887593711408240 ) ) ;
#5854 = EDGE_CURVE ( 'NONE', #10333, #13069, #2503, .T. ) ;
#5855 = ORIENTED_EDGE ( 'NONE', *, *, #2253, .T. ) ;
#5856 = CARTESIAN_POINT ( 'NONE',  ( -8.776279441628885181, -6.799038105676576293, -3.000000000000000888 ) ) ;
#5858 = CIRCLE ( 'NONE', #11948, 0.8999999999999998002 ) ;
#5857 = CARTESIAN_POINT ( 'NONE',  ( -8.632250723006720250, -18.84644399697197770, 13.00000000000000178 ) ) ;
#5859 = CYLINDRICAL_SURFACE ( 'NONE', #16025, 13.00000000000000178 ) ;
#5860 = CARTESIAN_POINT ( 'NONE',  ( 27.23057351405260818, -1.848475362037681480, -5.783357778048658027 ) ) ;
#5861 = PRESENTATION_LAYER_ASSIGNMENT (  '', '', ( #962 ) ) ;
#5862 = FACE_OUTER_BOUND ( 'NONE', #16136, .T. ) ;
#5863 = CARTESIAN_POINT ( 'NONE',  ( -2.016448651773435938E-27, -20.49999999999999645, 13.00000000000000178 ) ) ;
#5864 = CARTESIAN_POINT ( 'NONE',  ( 29.82181869931131146, -4.443908660051686610, -3.627061608673664672 ) ) ;
#5865 =( BOUNDED_SURFACE ( )  B_SPLINE_SURFACE ( 1, 2, ( 
 ( #16235, #10581, #5231, #16063, #6437, #2369, #6601, #16330, #8052, #14863, #2451, #2191, #9407, #3808, #2276, #14612, #13231, #14948, #7794, #11958, #808, #6340, #10753, #11864, #2525, #13591, #9326, #17442, #7973, #13421, #1078, #1173, #12225, #5060, #16148, #3709, #9232, #14782, #1000, #4329, #17881, #6957, #4062, #6785, #13765, #16489, #8314, #255, #8406, #2879, #14035, #5674, #9572, #11185, #9842, #16758, #15392, #11280, #6865, #15297, #5766, #5406, #2711, #12396, #12314, #8232, #1343, #13846, #17963, #15124, #5495, #10923, #11017, #2979, #12489, #74, #4163, #16578, #8502, #4244, #7153, #1434, #16858, #2618, #9659, #15209, #16671, #5586, #2791, #1624, #7065, #11103, #9744, #13938, #8147, #1532, #12663, #9491, #15031, #12583, #13678, #162, #1266, #4684, #8585, #7338, #6227, #14121, #17036, #7423, #352, #5860, #17135, #1710, #2075, #10212, #4508, #7599, #7241, #3419, #1981, #15761, #11748, #17231, #4594, #11383, #4771, #14314, #12757, #8687, #10022, #522, #13125, #12938, #10115, #11664, #13027, #15664, #1896, #3335, #8951, #16950, #445, #15570, #10295, #3150, #6037, #3244, #11567, #15845, #14214, #14398, #7505 ),
 ( #14492, #8865, #15485, #1808, #616, #12856, #5947, #704, #8781, #6137, #11471, #4422, #9934, #3066, #6316, #2252, #7770, #2171, #10562, #3511, #7864, #16127, #880, #3689, #13212, #9211, #976, #4949, #6502, #13395, #17417, #11930, #9042, #14672, #3611, #789, #14595, #15940, #12018, #14760, #9133, #7685, #17602, #2345, #16042, #10477, #11839, #13299, #6413, #17518, #5121, #5040, #17317, #4856, #10387, #12601, #6804, #8332, #8520, #1550, #15317, #9762, #11119, #2896, #8167, #273, #1362, #2999, #8425, #12510, #15230, #5603, #1641, #13866, #15146, #13961, #5786, #12415, #15052, #7083, #11205, #17896, #180, #16778, #15413, #10944, #5691, #2730, #4347, #9858, #1282, #14052, #9591, #7173, #12682, #2, #16427, #3992, #6887, #4263, #12331, #2808, #16601, #8251, #5427, #13699, #9508, #2639, #9679, #16508, #4079, #13784, #11036, #5517, #4180, #1452, #6981, #16688, #95, #693, #10010, #11652, #430, #5936, #17219, #1794, #2159, #4758, #4580, #7676, #8673, #3499, #2064, #11461, #10284, #7587, #9031, #15833, #17027, #13113, #14386, #511, #6217, #10103, #8770, #10202, #14480, #11735, #15928, #3406, #8938, #15556, #17308 ) ),
 .UNSPECIFIED., .F., .F., .T. ) 
 B_SPLINE_SURFACE_WITH_KNOTS ( ( 2, 2 ),
 ( 3, 2, 2, 2, 2, 2, 2, 2, 2, 2, 2, 2, 2, 2, 2, 2, 2, 2, 2, 2, 2, 2, 2, 2, 2, 2, 2, 2, 2, 2, 2, 2, 2, 2, 2, 2, 2, 2, 2, 2, 2, 2, 2, 2, 2, 2, 2, 2, 2, 2, 2, 2, 2, 2, 2, 2, 2, 2, 2, 2, 2, 2, 2, 2, 2, 2, 2, 2, 2, 2, 2, 2, 2, 2, 2, 2, 3 ),
 ( 0.000000000000000000, 1.000000000000000000 ),
 ( 0.000000000000000000, 0.01282051282051282007, 0.02564102564102564014, 0.03846153846153846367, 0.05128205128205128027, 0.06410256410256409687, 0.07692307692307692735, 0.08974358974358974395, 0.1025641025641025605, 0.1153846153846153910, 0.1282051282051281937, 0.1410256410256410242, 0.1538461538461538547, 0.1666666666666666574, 0.1794871794871794879, 0.1923076923076923184, 0.2051282051282051211, 0.2179487179487179516, 0.2307692307692307820, 0.2435897435897435848, 0.2564102564102563875, 0.2692307692307692180, 0.2820512820512820484, 0.2948717948717948789, 0.3076923076923077094, 0.3205128205128205399, 0.3333333333333333148, 0.3461538461538461453, 0.3589743589743589758, 0.3717948717948718063, 0.3846153846153846367, 0.3974358974358974117, 0.4102564102564102422, 0.4230769230769230727, 0.4358974358974359031, 0.4487179487179487336, 0.4615384615384615641, 0.4743589743589743390, 0.4871794871794871695, 0.5000000000000000000, 0.5128205128205127750, 0.5256410256410256610, 0.5384615384615384359, 0.5512820512820513219, 0.5641025641025640969, 0.5769230769230768718, 0.5897435897435897578, 0.6025641025641025328, 0.6153846153846154188, 0.6282051282051281937, 0.6410256410256410797, 0.6538461538461538547, 0.6666666666666666297, 0.6794871794871795156, 0.6923076923076922906, 0.7051282051282051766, 0.7179487179487179516, 0.7307692307692307265, 0.7435897435897436125, 0.7564102564102563875, 0.7692307692307692735, 0.7820512820512820484, 0.7948717948717948234, 0.8076923076923077094, 0.8205128205128204844, 0.8333333333333333703, 0.8461538461538461453, 0.8589743589743589203, 0.8717948717948718063, 0.8846153846153845812, 0.8974358974358974672, 0.9102564102564102422, 0.9230769230769231282, 0.9358974358974359031, 0.9487179487179486781, 0.9615384615384615641, 0.9690837704703162414 ),
 .UNSPECIFIED. ) 
 GEOMETRIC_REPRESENTATION_ITEM ( )  RATIONAL_B_SPLINE_SURFACE ( (
 ( 1.000000000000000000, 0.8660254037844387076, 1.000000000000000000, 0.8660254037844387076, 1.000000000000000000, 0.8660254037844387076, 1.000000000000000000, 0.8660254037844387076, 1.000000000000000000, 0.8660254037844387076, 1.000000000000000000, 0.8660254037844387076, 1.000000000000000000, 0.8660254037844387076, 1.000000000000000000, 0.8660254037844387076, 1.000000000000000000, 0.8660254037844387076, 1.000000000000000000, 0.8660254037844387076, 1.000000000000000000, 0.8660254037844387076, 1.000000000000000000, 0.8660254037844387076, 1.000000000000000000, 0.8660254037844387076, 1.000000000000000000, 0.8660254037844387076, 1.000000000000000000, 0.8660254037844387076, 1.000000000000000000, 0.8660254037844387076, 1.000000000000000000, 0.8660254037844387076, 1.000000000000000000, 0.8660254037844387076, 1.000000000000000000, 0.8660254037844387076, 1.000000000000000000, 0.8660254037844387076, 1.000000000000000000, 0.8660254037844387076, 1.000000000000000000, 0.8660254037844387076, 1.000000000000000000, 0.8660254037844387076, 1.000000000000000000, 0.8660254037844387076, 1.000000000000000000, 0.8660254037844387076, 1.000000000000000000, 0.8660254037844387076, 1.000000000000000000, 0.8660254037844387076, 1.000000000000000000, 0.8660254037844387076, 1.000000000000000000, 0.8660254037844387076, 1.000000000000000000, 0.8660254037844387076, 1.000000000000000000, 0.8660254037844387076, 1.000000000000000000, 0.8660254037844387076, 1.000000000000000000, 0.8660254037844387076, 1.000000000000000000, 0.8660254037844387076, 1.000000000000000000, 0.8660254037844387076, 1.000000000000000000, 0.8660254037844387076, 1.000000000000000000, 0.8660254037844387076, 1.000000000000000000, 0.8660254037844387076, 1.000000000000000000, 0.8660254037844387076, 1.000000000000000000, 0.8660254037844387076, 1.000000000000000000, 0.8660254037844387076, 1.000000000000000000, 0.8660254037844387076, 1.000000000000000000, 0.8660254037844387076, 1.000000000000000000, 0.8660254037844387076, 1.000000000000000000, 0.8660254037844387076, 1.000000000000000000, 0.8660254037844387076, 1.000000000000000000, 0.8660254037844387076, 1.000000000000000000, 0.8660254037844387076, 1.000000000000000000, 0.8660254037844387076, 1.000000000000000000, 0.8660254037844387076, 1.000000000000000000, 0.8660254037844387076, 1.000000000000000000, 0.8660254037844387076, 1.000000000000000000, 0.8660254037844387076, 1.000000000000000000, 0.8660254037844387076, 1.000000000000000000, 0.8660254037844387076, 1.000000000000000000, 0.8660254037844387076, 1.000000000000000000, 0.8660254037844387076, 1.000000000000000000, 0.8660254037844387076, 1.000000000000000000, 0.8660254037844387076, 1.000000000000000000, 0.8660254037844387076, 1.000000000000000000, 0.8660254037844387076, 1.000000000000000000, 0.8660254037844387076, 1.000000000000000000, 0.8660254037844387076, 1.000000000000000000, 0.8660254037844387076, 1.000000000000000000, 0.8660254037844387076, 1.000000000000000000, 0.8660254037844387076, 1.000000000000000000, 0.8660254037844387076, 1.000000000000000000, 0.8660254037844387076, 1.000000000000000000, 0.8660254037844387076, 1.000000000000000000, 0.8660254037844387076, 1.000000000000000000, 0.8660254037844387076, 1.000000000000000000, 0.8660254037844387076, 1.000000000000000000, 0.8660254037844387076, 1.000000000000000000, 0.8660254037844387076, 1.000000000000000000, 0.8660254037844387076, 1.000000000000000000, 0.9211513820375816231, 0.9351129643698559146),
 ( 1.000000000000000000, 0.8660254037844387076, 1.000000000000000000, 0.8660254037844387076, 1.000000000000000000, 0.8660254037844387076, 1.000000000000000000, 0.8660254037844387076, 1.000000000000000000, 0.8660254037844387076, 1.000000000000000000, 0.8660254037844387076, 1.000000000000000000, 0.8660254037844387076, 1.000000000000000000, 0.8660254037844387076, 1.000000000000000000, 0.8660254037844387076, 1.000000000000000000, 0.8660254037844387076, 1.000000000000000000, 0.8660254037844387076, 1.000000000000000000, 0.8660254037844387076, 1.000000000000000000, 0.8660254037844387076, 1.000000000000000000, 0.8660254037844387076, 1.000000000000000000, 0.8660254037844387076, 1.000000000000000000, 0.8660254037844387076, 1.000000000000000000, 0.8660254037844387076, 1.000000000000000000, 0.8660254037844387076, 1.000000000000000000, 0.8660254037844387076, 1.000000000000000000, 0.8660254037844387076, 1.000000000000000000, 0.8660254037844387076, 1.000000000000000000, 0.8660254037844387076, 1.000000000000000000, 0.8660254037844387076, 1.000000000000000000, 0.8660254037844387076, 1.000000000000000000, 0.8660254037844387076, 1.000000000000000000, 0.8660254037844387076, 1.000000000000000000, 0.8660254037844387076, 1.000000000000000000, 0.8660254037844387076, 1.000000000000000000, 0.8660254037844387076, 1.000000000000000000, 0.8660254037844387076, 1.000000000000000000, 0.8660254037844387076, 1.000000000000000000, 0.8660254037844387076, 1.000000000000000000, 0.8660254037844387076, 1.000000000000000000, 0.8660254037844387076, 1.000000000000000000, 0.8660254037844387076, 1.000000000000000000, 0.8660254037844387076, 1.000000000000000000, 0.8660254037844387076, 1.000000000000000000, 0.8660254037844387076, 1.000000000000000000, 0.8660254037844387076, 1.000000000000000000, 0.8660254037844387076, 1.000000000000000000, 0.8660254037844387076, 1.000000000000000000, 0.8660254037844387076, 1.000000000000000000, 0.8660254037844387076, 1.000000000000000000, 0.8660254037844387076, 1.000000000000000000, 0.8660254037844387076, 1.000000000000000000, 0.8660254037844387076, 1.000000000000000000, 0.8660254037844387076, 1.000000000000000000, 0.8660254037844387076, 1.000000000000000000, 0.8660254037844387076, 1.000000000000000000, 0.8660254037844387076, 1.000000000000000000, 0.8660254037844387076, 1.000000000000000000, 0.8660254037844387076, 1.000000000000000000, 0.8660254037844387076, 1.000000000000000000, 0.8660254037844387076, 1.000000000000000000, 0.8660254037844387076, 1.000000000000000000, 0.8660254037844387076, 1.000000000000000000, 0.8660254037844387076, 1.000000000000000000, 0.8660254037844387076, 1.000000000000000000, 0.8660254037844387076, 1.000000000000000000, 0.8660254037844387076, 1.000000000000000000, 0.8660254037844387076, 1.000000000000000000, 0.8660254037844387076, 1.000000000000000000, 0.8660254037844387076, 1.000000000000000000, 0.8660254037844387076, 1.000000000000000000, 0.8660254037844387076, 1.000000000000000000, 0.8660254037844387076, 1.000000000000000000, 0.8660254037844387076, 1.000000000000000000, 0.8660254037844387076, 1.000000000000000000, 0.8660254037844387076, 1.000000000000000000, 0.8660254037844387076, 1.000000000000000000, 0.8660254037844387076, 1.000000000000000000, 0.8660254037844387076, 1.000000000000000000, 0.8660254037844387076, 1.000000000000000000, 0.8660254037844387076, 1.000000000000000000, 0.8660254037844387076, 1.000000000000000000, 0.9211513820375816231, 0.9351129643698559146) ) ) 
 REPRESENTATION_ITEM ( '' )  SURFACE ( )  );
#5866 = DIRECTION ( 'NONE',  ( 0.000000000000000000, 0.000000000000000000, -1.000000000000000000 ) ) ;
#5867 = CARTESIAN_POINT ( 'NONE',  ( 26.79905070906539777, -3.354278923027479209, -3.283357778048662023 ) ) ;
#5868 = EDGE_CURVE ( 'NONE', #7716, #3354, #831, .T. ) ;
#5869 = TOROIDAL_SURFACE ( 'NONE', #16039, 3.199999999999998845, 0.8000000000000001554 ) ;
#5870 = ORIENTED_EDGE ( 'NONE', *, *, #13770, .T. ) ;
#5871 = ORIENTED_EDGE ( 'NONE', *, *, #1296, .T. ) ;
#5872 = ORIENTED_EDGE ( 'NONE', *, *, #9666, .F. ) ;
#5873 = CARTESIAN_POINT ( 'NONE',  ( 29.49337484321020497, -2.602568060005117090, 6.861505862736165362 ) ) ;
#5874 = DIRECTION ( 'NONE',  ( -0.9928203230275510771, -0.1196152422706610735, 0.000000000000000000 ) ) ;
#5875 = DIRECTION ( 'NONE',  ( -0.000000000000000000, -0.000000000000000000, -1.000000000000000000 ) ) ;
#5876 = DIRECTION ( 'NONE',  ( 1.000000000000000000, 0.000000000000000000, 0.000000000000000000 ) ) ;
#5877 = EDGE_CURVE ( 'NONE', #9127, #7301, #3146, .T. ) ;
#5878 = CARTESIAN_POINT ( 'NONE',  ( -5.781152949374542160, -1.605699403978851247, -1.901951201008075243 ) ) ;
#5880 = ADVANCED_FACE ( 'NONE', ( #17778 ), #10817, .F. ) ;
#5879 = CARTESIAN_POINT ( 'NONE',  ( 25.81100034576892455, -6.186289477007987259, -7.540293452860097112 ) ) ;
#5881 = DIRECTION ( 'NONE',  ( 0.9928203230275512992, 0.1196152422706614898, -0.000000000000000000 ) ) ;
#5882 = CARTESIAN_POINT ( 'NONE',  ( 45.50000000000000000, -19.03270077640483038, -5.537981825772250843 ) ) ;
#5883 = CARTESIAN_POINT ( 'NONE',  ( 0.6507732100473438974, -4.243078065514786168, -0.2236248678334921414 ) ) ;
#5884 = CARTESIAN_POINT ( 'NONE',  ( -10.78415792467453471, 15.55827129984638901, 16.70145112110344598 ) ) ;
#5885 = VERTEX_POINT ( 'NONE', #6763 ) ;
#5886 = CARTESIAN_POINT ( 'NONE',  ( 29.82181869931131146, -4.443908660051686610, -3.627061608673664672 ) ) ;
#5887 = CARTESIAN_POINT ( 'NONE',  ( 10.27627944162880702, -4.200961894323389956, -2.000000000000000000 ) ) ;
#5888 = CARTESIAN_POINT ( 'NONE',  ( 33.14105852333657509, -6.224726188408045147, -4.533357778048668685 ) ) ;
#5889 = CARTESIAN_POINT ( 'NONE',  ( 36.27615609941022257, -23.17738945083361557, 0.000000000000000000 ) ) ;
#5890 = ORIENTED_EDGE ( 'NONE', *, *, #12326, .F. ) ;
#5891 = CARTESIAN_POINT ( 'NONE',  ( 27.82847066025702887, -2.165988739474055791, 5.783357778048667797 ) ) ;
#5892 = EDGE_CURVE ( 'NONE', #118, #11309, #9553, .T. ) ;
#5893 = CARTESIAN_POINT ( 'NONE',  ( 29.91004888286193619, -6.613999042680076990, 7.033357778048657138 ) ) ;
#5894 = CARTESIAN_POINT ( 'NONE',  ( 26.36761712467744090, -6.740983333149474177, -4.705209693361168455 ) ) ;
#5895 = ORIENTED_EDGE ( 'NONE', *, *, #13074, .F. ) ;
#5896 = ORIENTED_EDGE ( 'NONE', *, *, #16346, .T. ) ;
#5897 = DIRECTION ( 'NONE',  ( 1.000000000000000000, 0.000000000000000000, 0.000000000000000000 ) ) ;
#5898 = LINE ( 'NONE', #15338, #1778 ) ;
#5899 = ADVANCED_FACE ( 'NONE', ( #5471 ), #499, .F. ) ;
#5900 = ORIENTED_EDGE ( 'NONE', *, *, #4484, .F. ) ;
#5901 = PRODUCT_DEFINITION ( 'UNKNOWN', '', #15858, #6844 ) ;
#5902 = CARTESIAN_POINT ( 'NONE',  ( 26.60838078660069428, -6.085005533777348319, -7.939653947423662927 ) ) ;
#5903 = VERTEX_POINT ( 'NONE', #16734 ) ;
#5904 = CARTESIAN_POINT ( 'NONE',  ( 32.02836186724004364, -4.178063784105134459, -7.939653947423662039 ) ) ;
#5905 = ORIENTED_EDGE ( 'NONE', *, *, #15558, .F. ) ;
#5906 = CYLINDRICAL_SURFACE ( 'NONE', #17445, 2.749999999999992006 ) ;
#5907 = CARTESIAN_POINT ( 'NONE',  ( 27.19802975513453092, -2.241944418315925613, -5.783357778048658027 ) ) ;
#5908 = CARTESIAN_POINT ( 'NONE',  ( 27.33945763453056088, -4.742984145595265488, 3.283357778048664244 ) ) ;
#5909 = CARTESIAN_POINT ( 'NONE',  ( 30.37154917142620292, -2.923863409590206519, -8.283357778048658915 ) ) ;
#5910 = CARTESIAN_POINT ( 'NONE',  ( -8.874038404635921751, 3.391377654146875642, -2.000000000000000000 ) ) ;
#5911 = ADVANCED_FACE ( 'NONE', ( #16927 ), #5651, .T. ) ;
#5912 = CARTESIAN_POINT ( 'NONE',  ( 33.28924367748503244, -4.026152426421394814, 3.627061608673664228 ) ) ;
#5913 =( GEOMETRIC_REPRESENTATION_CONTEXT ( 3 ) GLOBAL_UNCERTAINTY_ASSIGNED_CONTEXT ( ( #638 ) ) GLOBAL_UNIT_ASSIGNED_CONTEXT ( ( #792, #16216, #7688 ) ) REPRESENTATION_CONTEXT ( 'NONE', 'WORKASPACE' ) );
#5914 = CARTESIAN_POINT ( 'NONE',  ( -22.21647589440744142, -22.43199035874600966, 15.08811024704901094 ) ) ;
#5915 = DIRECTION ( 'NONE',  ( 0.9928203230275510771, 0.1196152422706614621, -0.000000000000000000 ) ) ;
#5916 = ADVANCED_FACE ( 'NONE', ( #4307 ), #3456, .F. ) ;
#5917 = ORIENTED_EDGE ( 'NONE', *, *, #3587, .T. ) ;
#5918 = DIRECTION ( 'NONE',  ( 0.9979201627913403261, -0.06446199418653547619, 0.000000000000000000 ) ) ;
#5919 = EDGE_LOOP ( 'NONE', ( #9185, #7628, #13149, #4915 ) ) ;
#5920 = DIRECTION ( 'NONE',  ( -0.000000000000000000, -0.000000000000000000, 1.000000000000000000 ) ) ;
#5921 = CARTESIAN_POINT ( 'NONE',  ( 25.93714794488954212, -2.393855775999666591, -5.783357778048658027 ) ) ;
#5922 = ORIENTED_EDGE ( 'NONE', *, *, #16179, .T. ) ;
#5923 = CARTESIAN_POINT ( 'NONE',  ( 13.00000000000000178, 0.000000000000000000, 10.50000000000000000 ) ) ;
#5924 = CARTESIAN_POINT ( 'NONE',  ( 33.95908713831676096, -3.945449517755638791, -3.283357778048664688 ) ) ;
#5925 = CARTESIAN_POINT ( 'NONE',  ( 26.01652455409633902, -4.902371455920926380, 5.783357778048663356 ) ) ;
#5926 = DIRECTION ( 'NONE',  ( 1.000000000000000000, 0.000000000000000000, 0.000000000000000000 ) ) ;
#5927 = DIRECTION ( 'NONE',  ( 0.000000000000000000, 0.000000000000000000, 0.9999999999999998890 ) ) ;
#5928 = LINE ( 'NONE', #7315, #15030 ) ;
#5929 = CARTESIAN_POINT ( 'NONE',  ( 28.52162355051263987, -6.481468097106410475, -6.861505862736167138 ) ) ;
#5930 = CARTESIAN_POINT ( 'NONE',  ( 33.76207435632690590, -3.969185667289998332, -3.627061608673664672 ) ) ;
#5931 = CARTESIAN_POINT ( 'NONE',  ( 26.01652455409633902, -4.902371455920928156, -5.783357778048663356 ) ) ;
#5932 = CARTESIAN_POINT ( 'NONE',  ( 33.78529456515154550, -6.484467084455913799, 5.783357778048664244 ) ) ;
#5933 = CARTESIAN_POINT ( 'NONE',  ( 30.29464937815318493, -4.386941900920275472, 3.627061608673664228 ) ) ;
#5934 = EDGE_CURVE ( 'NONE', #14281, #602, #7648, .T. ) ;
#5935 = ORIENTED_EDGE ( 'NONE', *, *, #1268, .F. ) ;
#5936 = CARTESIAN_POINT ( 'NONE',  ( 26.84461768998868436, -2.294720455324902542, -5.783357778048658027 ) ) ;
#5937 = ORIENTED_EDGE ( 'NONE', *, *, #17446, .T. ) ;
#5938 = CARTESIAN_POINT ( 'NONE',  ( 27.47505859511117521, -2.218764776483033163, 5.783357778048668685 ) ) ;
#5939 = CARTESIAN_POINT ( 'NONE',  ( 31.71807556108801407, -1.697368162559112825, -5.113484796970855228 ) ) ;
#5940 = FACE_OUTER_BOUND ( 'NONE', #12125, .T. ) ;
#5941 = EDGE_CURVE ( 'NONE', #17858, #14967, #17065, .T. ) ;
#5942 = ORIENTED_EDGE ( 'NONE', *, *, #15442, .T. ) ;
#5943 = CARTESIAN_POINT ( 'NONE',  ( 28.05993251931039012, -3.202367565343740452, -3.283357778048662023 ) ) ;
#5944 = CARTESIAN_POINT ( 'NONE',  ( 27.55969062878875064, -7.234529412811931515, 5.783357778048657138 ) ) ;
#5945 = DIRECTION ( 'NONE',  ( -0.9928203230275510771, -0.1196152422706614760, -0.000000000000000000 ) ) ;
#5946 = CARTESIAN_POINT ( 'NONE',  ( 27.45273115869273539, -7.247415916675651992, -5.113484796970856117 ) ) ;
#5947 = CARTESIAN_POINT ( 'NONE',  ( 33.28924367748503244, -4.026152426421394814, -7.939653947423662039 ) ) ;
#5948 = CARTESIAN_POINT ( 'NONE',  ( -3.538288549924106796, -15.34800872113743431, 16.99955934415556769 ) ) ;
#5949 = CARTESIAN_POINT ( 'NONE',  ( 3.347071143357317702, -15.22052928361023127, 17.00000000000000000 ) ) ;
#5950 = CARTESIAN_POINT ( 'NONE',  ( 32.16857880351144416, -6.669052543620333395, -5.783357778048668685 ) ) ;
#5951 = CARTESIAN_POINT ( 'NONE',  ( 28.72797218747911074, -6.756415940301135237, 7.033357778048657138 ) ) ;
#5952 = CARTESIAN_POINT ( 'NONE',  ( 29.89119874204131122, -2.254829357712824667, 7.033357778048666020 ) ) ;
#5953 = ADVANCED_FACE ( 'NONE', ( #6627 ), #16356, .F. ) ;
#5954 = EDGE_LOOP ( 'NONE', ( #16727, #649, #6029 ) ) ;
#5955 = ORIENTED_EDGE ( 'NONE', *, *, #3783, .F. ) ;
#5956 = EDGE_LOOP ( 'NONE', ( #2610, #8390, #11440, #4198, #12672 ) ) ;
#5957 = CARTESIAN_POINT ( 'NONE',  ( 29.41022140756759029, -3.239556939666760726, 3.627061608673666449 ) ) ;
#5958 = EDGE_CURVE ( 'NONE', #6735, #475, #1113, .T. ) ;
#5959 = CARTESIAN_POINT ( 'NONE',  ( 29.08935247050201767, -2.014077381790315702, -5.783357778048658027 ) ) ;
#5960 = CARTESIAN_POINT ( 'NONE',  ( 26.31321956127059636, -7.341867041618697520, 5.319444967946814096 ) ) ;
#5961 = DIRECTION ( 'NONE',  ( -0.6000000000000000888, 0.7999999999999999334, 0.000000000000000000 ) ) ;
#5962 = CARTESIAN_POINT ( 'NONE',  ( -23.83685604381143364, -22.42490655540755284, -14.74319968589249719 ) ) ;
#5963 = CARTESIAN_POINT ( 'NONE',  ( 33.54323074294813267, -5.249493066516778050, -7.939653947423664704 ) ) ;
#5964 = CARTESIAN_POINT ( 'NONE',  ( -2.855764796983341736, 2.970025579236416302, -0.09382832055445670949 ) ) ;
#5965 = DIRECTION ( 'NONE',  ( -0.000000000000000000, 1.000000000000000000, 0.000000000000000000 ) ) ;
#5966 = CARTESIAN_POINT ( 'NONE',  ( 27.19802975513453092, -2.241944418315925613, -5.783357778048658027 ) ) ;
#5967 = CARTESIAN_POINT ( 'NONE',  ( 38.62156597043018991, -0.8438693783906362489, -3.150911402496571867 ) ) ;
#5968 =( BOUNDED_CURVE ( )  B_SPLINE_CURVE ( 2, ( #3379, #4909, #3296, #572, #11797, #4643, #1943, #17184, #7554 ),
 .UNSPECIFIED., .F., .F. ) 
 B_SPLINE_CURVE_WITH_KNOTS ( ( 3, 2, 2, 2, 3 ),
 ( 0.01923076923076924918, 0.02564102564102564014, 0.03846153846153846367, 0.05128205128205128027, 0.05769230769230770939 ),
 .UNSPECIFIED. ) 
 CURVE ( )  GEOMETRIC_REPRESENTATION_ITEM ( )  RATIONAL_B_SPLINE_CURVE ( ( 0.9330127018922194093, 0.9330127018922195203, 1.000000000000000000, 0.8660254037844387076, 1.000000000000000000, 0.8660254037844387076, 1.000000000000000000, 0.9330127018922190762, 0.9330127018922194093 ) ) 
 REPRESENTATION_ITEM ( '' )  );
#5969 = ADVANCED_FACE ( 'NONE', ( #4090 ), #16783, .F. ) ;
#5970 = DIRECTION ( 'NONE',  ( -0.000000000000000000, -0.000000000000000000, 1.000000000000000000 ) ) ;
#5971 = EDGE_LOOP ( 'NONE', ( #5905, #4759, #4781, #8990 ) ) ;
#5972 = CARTESIAN_POINT ( 'NONE',  ( 27.09860475545177039, -3.518061095420291995, -3.627061608673662896 ) ) ;
#5973 = FACE_OUTER_BOUND ( 'NONE', #200, .T. ) ;
#5974 = LINE ( 'NONE', #8810, #17329 ) ;
#5975 = DIRECTION ( 'NONE',  ( -0.5000000000000099920, -0.8660254037844329345, 0.000000000000000000 ) ) ;
#5976 = CARTESIAN_POINT ( 'NONE',  ( 28.64916707261694384, -6.765910400363817523, 7.033357778048657138 ) ) ;
#5977 = CARTESIAN_POINT ( 'NONE',  ( 28.69037342443288452, -3.126411886501869741, 8.283357778048664244 ) ) ;
#5978 = CARTESIAN_POINT ( 'NONE',  ( 26.98483462626008134, -4.785709214840094816, -7.939653947423662039 ) ) ;
#5979 = ORIENTED_EDGE ( 'NONE', *, *, #7750, .T. ) ;
#5980 = CARTESIAN_POINT ( 'NONE',  ( 26.70901672940806648, -4.818939824437135755, 3.283357778048664244 ) ) ;
#5981 = VERTEX_POINT ( 'NONE', #16515 ) ;
#5982 = ORIENTED_EDGE ( 'NONE', *, *, #6828, .F. ) ;
#5983 = CARTESIAN_POINT ( 'NONE',  ( 29.42969845347704450, -5.944964990802679594, -8.283357778048664244 ) ) ;
#5984 = EDGE_LOOP ( 'NONE', ( #13664, #5464 ) ) ;
#5985 = PRODUCT_DEFINITION_FORMATION_WITH_SPECIFIED_SOURCE ( 'ANY', '', #15045, .NOT_KNOWN. ) ;
#5986 = CARTESIAN_POINT ( 'NONE',  ( 27.65911562847151117, -5.958412735707574015, -3.627061608673668225 ) ) ;
#5987 = EDGE_CURVE ( 'NONE', #254, #14093, #264, .T. ) ;
#5988 = CARTESIAN_POINT ( 'NONE',  ( 27.26074174026764751, -6.633379454790151009, -6.861505862736167138 ) ) ;
#5989 = VECTOR ( 'NONE', #17093, 1000.000000000000000 ) ;
#5990 = CARTESIAN_POINT ( 'NONE',  ( 30.86385689617752348, -5.572304701594726239, -7.939653947423664704 ) ) ;
#5991 = ORIENTED_EDGE ( 'NONE', *, *, #7093, .F. ) ;
#5992 = DIRECTION ( 'NONE',  ( -0.000000000000000000, -0.000000000000000000, -1.000000000000000000 ) ) ;
#5993 = CARTESIAN_POINT ( 'NONE',  ( 29.14074637024071990, -5.979778010479330774, -3.283357778048667797 ) ) ;
#5994 = DIRECTION ( 'NONE',  ( 0.7999999999999999334, 0.6000000000000001998, 0.000000000000000000 ) ) ;
#5995 = ORIENTED_EDGE ( 'NONE', *, *, #3739, .T. ) ;
#5996 = CARTESIAN_POINT ( 'NONE',  ( 32.50309786422735669, -5.574681056656012323, -8.283357778048662468 ) ) ;
#5997 = CARTESIAN_POINT ( 'NONE',  ( 3.248936832696173393, -28.97437970944926633, 17.00000000000000000 ) ) ;
#5998 = CARTESIAN_POINT ( 'NONE',  ( 33.40754056521197413, -5.892811586081919906, 4.705209693361160461 ) ) ;
#5999 = AXIS2_PLACEMENT_3D ( 'NONE', #15806, #3380, #8988 ) ;
#6000 = DIRECTION ( 'NONE',  ( 1.000000000000000000, 0.000000000000000000, -0.000000000000000000 ) ) ;
#6001 = CARTESIAN_POINT ( 'NONE',  ( -19.22707546753401786, -21.21757778339487288, 15.64731278403363035 ) ) ;
#6002 = CARTESIAN_POINT ( 'NONE',  ( -35.74085044863416272, -28.97437970944926988, 11.27079897466147607 ) ) ;
#6003 = ORIENTED_EDGE ( 'NONE', *, *, #2262, .T. ) ;
#6004 = LINE ( 'NONE', #10182, #14579 ) ;
#6005 = ORIENTED_EDGE ( 'NONE', *, *, #6900, .F. ) ;
#6006 = DIRECTION ( 'NONE',  ( 0.000000000000000000, 0.000000000000000000, -1.000000000000000000 ) ) ;
#6007 = CARTESIAN_POINT ( 'NONE',  ( -20.00000000000000000, 7.999999999999996447, 15.51150668642334374 ) ) ;
#6008 = EDGE_CURVE ( 'NONE', #16863, #11660, #16021, .T. ) ;
#6009 = ORIENTED_EDGE ( 'NONE', *, *, #307, .F. ) ;
#6010 = CARTESIAN_POINT ( 'NONE',  ( 23.02601376483258022, 3.965314980223224151, -6.000000000000000000 ) ) ;
#6011 = EDGE_CURVE ( 'NONE', #13121, #11972, #7798, .T. ) ;
#6012 = AXIS2_PLACEMENT_3D ( 'NONE', #15788, #11600, #6260 ) ;
#6013 = CARTESIAN_POINT ( 'NONE',  ( 32.41296236253129592, -1.951006642345344044, -4.533357778048659803 ) ) ;
#6014 = CYLINDRICAL_SURFACE ( 'NONE', #9267, 6.249999999999996447 ) ;
#6015 = DIRECTION ( 'NONE',  ( 0.000000000000000000, 0.000000000000000000, 1.000000000000000000 ) ) ;
#6016 = PLANE ( 'NONE',  #16204 ) ;
#6017 = CARTESIAN_POINT ( 'NONE',  ( 32.72003615946069743, -2.840789625746940938, -7.939653947423660263 ) ) ;
#6018 = AXIS2_PLACEMENT_3D ( 'NONE', #9357, #9182, #92 ) ;
#6019 = DIRECTION ( 'NONE',  ( 0.1195020427801297691, -0.9918807541847894926, 0.04349518650597276187 ) ) ;
#6021 = PLANE ( 'NONE',  #3722 ) ;
#6020 = AXIS2_PLACEMENT_3D ( 'NONE', #3495, #14195, #11546 ) ;
#6022 = CARTESIAN_POINT ( 'NONE',  ( 31.66930131758986988, -2.967382423816733894, 7.939653947423664704 ) ) ;
#6023 = ORIENTED_EDGE ( 'NONE', *, *, #17256, .T. ) ;
#6024 = CARTESIAN_POINT ( 'NONE',  ( 26.17715024865823281, -6.235583268514393929, 7.666572473558731282 ) ) ;
#6025 = ORIENTED_EDGE ( 'NONE', *, *, #9596, .F. ) ;
#6026 = CARTESIAN_POINT ( 'NONE',  ( 33.54323074294813267, -5.249493066516778050, 3.627061608673662896 ) ) ;
#6027 = CARTESIAN_POINT ( 'NONE',  ( 32.51061761821408425, -6.300681867249914525, -4.533357778048668685 ) ) ;
#6028 = DIRECTION ( 'NONE',  ( -1.000000000000000000, 0.000000000000000000, 0.000000000000000000 ) ) ;
#6029 = ORIENTED_EDGE ( 'NONE', *, *, #6464, .F. ) ;
#6030 = FACE_OUTER_BOUND ( 'NONE', #15171, .T. ) ;
#6031 = B_SPLINE_CURVE_WITH_KNOTS ( 'NONE', 3,
 ( #3779, #4858, #15941, #17603 ),
 .UNSPECIFIED., .F., .F.,
 ( 4, 4 ),
 ( 0.000000000000000000, 0.002452478801916362864 ),
 .UNSPECIFIED. ) ;
#6032 = AXIS2_PLACEMENT_3D ( 'NONE', #9213, #977, #7600 ) ;
#6033 = DIRECTION ( 'NONE',  ( 0.05980762113533059920, -0.4964101615137756496, -0.8660254037844385966 ) ) ;
#6034 = ORIENTED_EDGE ( 'NONE', *, *, #13553, .F. ) ;
#6035 = LINE ( 'NONE', #7421, #14552 ) ;
#6036 = CARTESIAN_POINT ( 'NONE',  ( 32.83754810739939956, -9.116730809865838836, 5.783357778048664244 ) ) ;
#6038 = ADVANCED_FACE ( 'NONE', ( #9598 ), #1573, .F. ) ;
#6037 = CARTESIAN_POINT ( 'NONE',  ( 25.47811240618384687, -2.786519109605914757, -4.533357778048659803 ) ) ;
#6039 = CARTESIAN_POINT ( 'NONE',  ( 33.04340326765378677, -1.875050963503474222, -4.533357778048659803 ) ) ;
#6040 = DIRECTION ( 'NONE',  ( -0.000000000000000000, -0.000000000000000000, -1.000000000000000000 ) ) ;
#6041 = FILL_AREA_STYLE ('',( #11284 ) ) ;
#6042 = CARTESIAN_POINT ( 'NONE',  ( 26.99805802979993885, -6.665027654307603022, -4.705209693361168455 ) ) ;
#6043 = EDGE_CURVE ( 'NONE', #3987, #15092, #13167, .T. ) ;
#6044 = CARTESIAN_POINT ( 'NONE',  ( 27.15566825608056689, -6.646038734597135011, -4.705209693361169343 ) ) ;
#6045 = CARTESIAN_POINT ( 'NONE',  ( 31.78252145740879797, -2.026962321187214311, 7.033357778048666020 ) ) ;
#6046 = AXIS2_PLACEMENT_3D ( 'NONE', #4918, #8070, #2040 ) ;
#6047 = ORIENTED_EDGE ( 'NONE', *, *, #17295, .T. ) ;
#6048 = ORIENTED_EDGE ( 'NONE', *, *, #17743, .T. ) ;
#6049 = VERTEX_POINT ( 'NONE', #7796 ) ;
#6050 = CARTESIAN_POINT ( 'NONE',  ( 27.02423718196931546, -4.780961985016209503, 8.283357778048662468 ) ) ;
#6051 = DIRECTION ( 'NONE',  ( 0.000000000000000000, 0.000000000000000000, 1.000000000000000000 ) ) ;
#6052 =( BOUNDED_CURVE ( )  B_SPLINE_CURVE ( 2, ( #4815, #12988, #11334, #485, #5908, #6186, #11708, #16912, #14168 ),
 .UNSPECIFIED., .F., .T. ) 
 B_SPLINE_CURVE_WITH_KNOTS ( ( 3, 2, 2, 2, 3 ),
 ( 0.7884615384615384359, 0.7948717948717948234, 0.8076923076923077094, 0.8205128205128204844, 0.8269230769230769829 ),
 .UNSPECIFIED. ) 
 CURVE ( )  GEOMETRIC_REPRESENTATION_ITEM ( )  RATIONAL_B_SPLINE_CURVE ( ( 0.9330127018922194093, 0.9330127018922194093, 1.000000000000000000, 0.8660254037844387076, 1.000000000000000000, 0.8660254037844387076, 1.000000000000000000, 0.9330127018922187432, 0.9330127018922192983 ) ) 
 REPRESENTATION_ITEM ( '' )  );
#6053 = DIRECTION ( 'NONE',  ( -0.7999999999999999334, -0.6000000000000001998, 0.000000000000000000 ) ) ;
#6054 = CARTESIAN_POINT ( 'NONE',  ( 0.000000000000000000, 0.000000000000000000, -3.000000000000002665 ) ) ;
#6055 = DIRECTION ( 'NONE',  ( -5.026720092345836698E-22, 4.581671729415424240E-22, -1.000000000000000000 ) ) ;
#6056 = CARTESIAN_POINT ( 'NONE',  ( 32.29974222271236073, -2.891426744974864071, -3.627061608673662008 ) ) ;
#6057 = CARTESIAN_POINT ( 'NONE',  ( 31.32102116884452414, -5.717097954277069682, -8.283357778048664244 ) ) ;
#6058 = CARTESIAN_POINT ( 'NONE',  ( 25.71748644841968456, -2.420320648352046078, 5.783357778048663356 ) ) ;
#6059 = ORIENTED_EDGE ( 'NONE', *, *, #6971, .T. ) ;
#6060 = AXIS2_PLACEMENT_3D ( 'NONE', #6687, #12220, #12310 ) ;
#6062 = EDGE_CURVE ( 'NONE', #15290, #558, #14354, .T. ) ;
#6061 = CARTESIAN_POINT ( 'NONE',  ( 45.00000000000000711, -16.03270077640482683, -5.537981825772250843 ) ) ;
#6063 = DIRECTION ( 'NONE',  ( -1.224646799147353207E-16, 1.000000000000000000, 0.000000000000000000 ) ) ;
#6064 = CARTESIAN_POINT ( 'NONE',  ( 26.75784435724945709, -6.993777436889428323, -4.533357778048668685 ) ) ;
#6065 = ORIENTED_EDGE ( 'NONE', *, *, #9691, .F. ) ;
#6066 = VERTEX_POINT ( 'NONE', #7458 ) ;
#6067 = CARTESIAN_POINT ( 'NONE',  ( 25.77727992838053339, -5.625024813964539128, -7.939653947423662927 ) ) ;
#6068 = CARTESIAN_POINT ( 'NONE',  ( 30.42903939560917337, -1.852671564043892660, -5.783357778048658027 ) ) ;
#6069 = CARTESIAN_POINT ( 'NONE',  ( -8.812506826975363694, -18.97024042328638416, 16.83711976780714181 ) ) ;
#6070 = CARTESIAN_POINT ( 'NONE',  ( 26.04653150877178902, -5.151432644682725659, -3.575219446611406227 ) ) ;
#6071 = AXIS2_PLACEMENT_3D ( 'NONE', #11750, #15942, #13127 ) ;
#6072 = EDGE_CURVE ( 'NONE', #4832, #1869, #2309, .T. ) ;
#6073 = DIRECTION ( 'NONE',  ( -0.9928203230275510771, -0.1196152422706614760, -0.000000000000000000 ) ) ;
#6074 = CARTESIAN_POINT ( 'NONE',  ( 28.48022645605872327, -3.151730446115816875, 3.283357778048666464 ) ) ;
#6075 = VECTOR ( 'NONE', #319, 1000.000000000000000 ) ;
#6076 = ORIENTED_EDGE ( 'NONE', *, *, #8060, .F. ) ;
#6077 = CARTESIAN_POINT ( 'NONE',  ( 4.000000000000000000, 2.309401076758510918, -0.5000000000000000000 ) ) ;
#6078 = CARTESIAN_POINT ( 'NONE',  ( 32.54503264317084188, -5.369756224683081669, -3.627061608673667781 ) ) ;
#6079 = ORIENTED_EDGE ( 'NONE', *, *, #13273, .F. ) ;
#6080 =( BOUNDED_CURVE ( )  B_SPLINE_CURVE ( 3, ( #16107, #3669, #5280, #1042 ),
 .UNSPECIFIED., .F., .T. ) 
 B_SPLINE_CURVE_WITH_KNOTS ( ( 4, 4 ),
 ( 5.052230418047667371, 5.061454830783549852 ),
 .UNSPECIFIED. ) 
 CURVE ( )  GEOMETRIC_REPRESENTATION_ITEM ( )  RATIONAL_B_SPLINE_CURVE ( ( 1.000000000000000000, 0.9999929091967096895, 0.9999929091967096895, 1.000000000000000000 ) ) 
 REPRESENTATION_ITEM ( '' )  );
#6081 = DIRECTION ( 'NONE',  ( 0.000000000000000000, -1.000000000000000000, -3.469446951953614189E-16 ) ) ;
#6082 = COLOUR_RGB ( '', 0.08235294, 0.09019608, 0.10196078) ;
#6083 = CARTESIAN_POINT ( 'NONE',  ( -23.00000000000000000, -16.21813761408365195, 13.00000000000000178 ) ) ;
#6084 = EDGE_CURVE ( 'NONE', #1473, #2720, #9327, .T. ) ;
#6085 = CARTESIAN_POINT ( 'NONE',  ( 25.86833963875586306, -3.039313213345869791, -4.705209693361160461 ) ) ;
#6086 = ORIENTED_EDGE ( 'NONE', *, *, #9838, .T. ) ;
#6087 = CARTESIAN_POINT ( 'NONE',  ( 25.96861057204955259, -6.167300557297518360, -7.540293452860097112 ) ) ;
#6088 = ORIENTED_EDGE ( 'NONE', *, *, #17358, .T. ) ;
#6089 = CARTESIAN_POINT ( 'NONE',  ( 26.87106449706838873, -6.053357334259913181, -3.627061608673667781 ) ) ;
#6090 = CARTESIAN_POINT ( 'NONE',  ( 28.69037342443288452, -3.126411886501869741, -3.283357778048662023 ) ) ;
#6091 = DIRECTION ( 'NONE',  ( -0.000000000000000000, 0.000000000000000000, 1.000000000000000000 ) ) ;
#6092 = EDGE_LOOP ( 'NONE', ( #7675, #6009 ) ) ;
#6093 = CARTESIAN_POINT ( 'NONE',  ( 29.67353201968042598, -1.554147106732884920, -5.783357778048658027 ) ) ;
#6094 = LINE ( 'NONE', #14551, #10038 ) ;
#6095 = CARTESIAN_POINT ( 'NONE',  ( 25.33925079868512498, -2.076342398563292058, 5.783357778048668685 ) ) ;
#6096 = AXIS2_PLACEMENT_3D ( 'NONE', #14470, #16106, #11642 ) ;
#6097 = EDGE_CURVE ( 'NONE', #10514, #11624, #4728, .T. ) ;
#6098 = VECTOR ( 'NONE', #7793, 1000.000000000000000 ) ;
#6099 = ORIENTED_EDGE ( 'NONE', *, *, #16567, .F. ) ;
#6100 = CARTESIAN_POINT ( 'NONE',  ( -13.00000000000000178, 1.592040838891559293E-15, -10.50000000000000000 ) ) ;
#6101 = PLANE ( 'NONE',  #2052 ) ;
#6102 = CARTESIAN_POINT ( 'NONE',  ( 23.00000000000000000, -16.21813761408365195, -13.00000000000000178 ) ) ;
#6103 = ORIENTED_EDGE ( 'NONE', *, *, #4015, .T. ) ;
#6104 = CARTESIAN_POINT ( 'NONE',  ( 1.500000000000000666, 5.809475019311125976, -1.901951201008075243 ) ) ;
#6105 = ORIENTED_EDGE ( 'NONE', *, *, #2930, .T. ) ;
#6106 = CARTESIAN_POINT ( 'NONE',  ( -9.749999999999953815, 3.897114317030088149, -3.000000000000000000 ) ) ;
#6107 = DIRECTION ( 'NONE',  ( 0.7999999999999999334, -0.6000000000000001998, 0.000000000000000000 ) ) ;
#6108 = ORIENTED_EDGE ( 'NONE', *, *, #14588, .T. ) ;
#6109 = CARTESIAN_POINT ( 'NONE',  ( 26.95740407890011170, -7.307093047852763590, -6.453230759126468818 ) ) ;
#6111 = EDGE_CURVE ( 'NONE', #8674, #11419, #7584, .T. ) ;
#6110 = AXIS2_PLACEMENT_3D ( 'NONE', #9339, #16507, #13698 ) ;
#6112 = AXIS2_PLACEMENT_3D ( 'NONE', #1352, #1183, #16589 ) ;
#6113 = CARTESIAN_POINT ( 'NONE',  ( 30.45035428628836627, -2.914368949527523789, -8.283357778048658915 ) ) ;
#6114 = DIRECTION ( 'NONE',  ( 0.6000000000000001998, 0.7999999999999999334, 0.000000000000000000 ) ) ;
#6115 = CARTESIAN_POINT ( 'NONE',  ( 46.86575133767495061, -2.390451368237048513, -5.783357778048661579 ) ) ;
#6116 = ORIENTED_EDGE ( 'NONE', *, *, #14797, .T. ) ;
#6117 = AXIS2_PLACEMENT_3D ( 'NONE', #4101, #2746, #8267 ) ;
#6118 = CARTESIAN_POINT ( 'NONE',  ( -25.74999999999999645, -16.21813761408365195, 0.000000000000000000 ) ) ;
#6119 = CARTESIAN_POINT ( 'NONE',  ( 31.80137159822941939, -6.386132006154467078, -4.533357778048668685 ) ) ;
#6120 = CARTESIAN_POINT ( 'NONE',  ( 27.67650891848073158, -3.448435056481901295, 3.627061608673666893 ) ) ;
#6121 = EDGE_CURVE ( 'NONE', #15406, #14372, #14753, .T. ) ;
#6122 = ORIENTED_EDGE ( 'NONE', *, *, #16472, .F. ) ;
#6123 = CARTESIAN_POINT ( 'NONE',  ( 26.31176419598820360, -7.352894575460818594, 5.384699358761103838 ) ) ;
#6124 = ORIENTED_EDGE ( 'NONE', *, *, #11306, .F. ) ;
#6125 = CARTESIAN_POINT ( 'NONE',  ( 25.58373587974369201, -2.446631813008643075, 5.783357778048668685 ) ) ;
#6126 = CARTESIAN_POINT ( 'NONE',  ( -28.91489957058744409, -14.18850833160549207, 13.46727466850441601 ) ) ;
#6127 = DIRECTION ( 'NONE',  ( 0.9928203230275510771, 0.1196152422706609902, 4.006172263299092517E-17 ) ) ;
#6128 = EDGE_LOOP ( 'NONE', ( #16808, #4013, #694 ) ) ;
#6129 = B_SPLINE_CURVE_WITH_KNOTS ( 'NONE', 3,
 ( #93, #9760, #1548, #13697, #11117, #7081, #5689, #1280, #2894, #3990, #1451, #9589, #17967, #4178, #15050, #4345 ),
 .UNSPECIFIED., .F., .F.,
 ( 4, 2, 2, 2, 2, 2, 2, 4 ),
 ( 0.000000000000000000, 0.0008414457502979328513, 0.001262168625446899277, 0.001682891500595865703, 0.002103614375744832128, 0.002524337250893798554, 0.002945060126042764979, 0.003365783001191731405 ),
 .UNSPECIFIED. ) ;
#6130 = CARTESIAN_POINT ( 'NONE',  ( 28.74176732417158320, -7.092112515190875044, -5.783357778048657138 ) ) ;
#6131 = VECTOR ( 'NONE', #4374, 1000.000000000000000 ) ;
#6132 = CARTESIAN_POINT ( 'NONE',  ( -4.211399291375529153, 2.459730787265042462, -3.451162385478148131 ) ) ;
#6133 = DIRECTION ( 'NONE',  ( -0.000000000000000000, -0.000000000000000000, 1.000000000000000000 ) ) ;
#6134 = ADVANCED_FACE ( 'NONE', ( #9661 ), #4065, .F. ) ;
#6135 = CARTESIAN_POINT ( 'NONE',  ( -1.999999999999999556, 3.464101615137755719, -2.842992957459236525 ) ) ;
#6136 = PRODUCT_RELATED_PRODUCT_CATEGORY ( 'part', '', ( #8245 ) ) ;
#6137 = CARTESIAN_POINT ( 'NONE',  ( 33.42946061375642586, -6.517141185936593750, -5.783357778048668685 ) ) ;
#6138 = CARTESIAN_POINT ( 'NONE',  ( -1.243833333691421572, 3.900674643483235560, -2.923144239647432752 ) ) ;
#6139 = VECTOR ( 'NONE', #6522, 1000.000000000000000 ) ;
#6140 = CARTESIAN_POINT ( 'NONE',  ( -12.50000000000000000, 0.000000000000000000, -4.000000000000000000 ) ) ;
#6141 = SHAPE_DEFINITION_REPRESENTATION ( #16218, #3227 ) ;
#6142 = CARTESIAN_POINT ( 'NONE',  ( 29.19137779418881351, -4.519864338893556877, -3.627061608673664672 ) ) ;
#6143 = ORIENTED_EDGE ( 'NONE', *, *, #15089, .T. ) ;
#6144 = LINE ( 'NONE', #5129, #2629 ) ;
#6145 = AXIS2_PLACEMENT_3D ( 'NONE', #10547, #17301, #2329 ) ;
#6146 = CARTESIAN_POINT ( 'NONE',  ( 32.34167700165585302, -2.686501913001913433, 3.283357778048666464 ) ) ;
#6147 = VECTOR ( 'NONE', #4005, 1000.000000000000000 ) ;
#6148 = EDGE_CURVE ( 'NONE', #9205, #14231, #1968, .T. ) ;
#6149 = VERTEX_POINT ( 'NONE', #2713 ) ;
#6150 = ORIENTED_EDGE ( 'NONE', *, *, #8192, .T. ) ;
#6151 = ORIENTED_EDGE ( 'NONE', *, *, #6329, .F. ) ;
#6152 = CARTESIAN_POINT ( 'NONE',  ( 26.88845778707760914, -3.543379655034240905, 3.627061608673666449 ) ) ;
#6153 = CIRCLE ( 'NONE', #2957, 0.9000000000000003553 ) ;
#6154 = CARTESIAN_POINT ( 'NONE',  ( 32.81641299864316608, -4.083119185552795294, 3.627061608673664228 ) ) ;
#6155 = CARTESIAN_POINT ( 'NONE',  ( -11.16099250167134826, 15.37423824781781079, -16.67067991271537863 ) ) ;
#6156 = CARTESIAN_POINT ( 'NONE',  ( -28.92121476417970882, -18.25996810291579209, -13.46562832783231478 ) ) ;
#6157 = CARTESIAN_POINT ( 'NONE',  ( 25.62757597683262034, -3.695291012717980994, -7.939653947423660263 ) ) ;
#6158 = CARTESIAN_POINT ( 'NONE',  ( 33.40745134805642635, -4.011910736534825439, -3.283357778048664688 ) ) ;
#6159 = EDGE_CURVE ( 'NONE', #2839, #7960, #12398, .T. ) ;
#6160 = CARTESIAN_POINT ( 'NONE',  ( -27.17934203385504333, -30.00000000000000355, -12.00000000000000000 ) ) ;
#6161 = VECTOR ( 'NONE', #14923, 1000.000000000000000 ) ;
#6162 = VECTOR ( 'NONE', #13108, 1000.000000000000000 ) ;
#6163 = CARTESIAN_POINT ( 'NONE',  ( 2.500000000000000000, 0.000000000000000000, 0.000000000000000000 ) ) ;
#6164 = CARTESIAN_POINT ( 'NONE',  ( 31.20090818012769773, -4.277755612481361602, -8.283357778048662468 ) ) ;
#6165 = CARTESIAN_POINT ( 'NONE',  ( -12.50000000000000000, 0.000000000000000000, -10.47749643873921244 ) ) ;
#6166 = EDGE_LOOP ( 'NONE', ( #308, #2339, #7470 ) ) ;
#6167 = CARTESIAN_POINT ( 'NONE',  ( 25.58373587974369201, -2.446631813008643075, -5.783357778048658027 ) ) ;
#6168 = DIRECTION ( 'NONE',  ( 0.000000000000000000, 0.000000000000000000, 1.000000000000000000 ) ) ;
#6169 = VERTEX_POINT ( 'NONE', #2793 ) ;
#6170 = DIRECTION ( 'NONE',  ( 1.000000000000000000, 0.000000000000000000, 0.000000000000000000 ) ) ;
#6171 = CARTESIAN_POINT ( 'NONE',  ( 28.01872616749444944, -6.841866079205687790, 7.033357778048657138 ) ) ;
#6172 = ADVANCED_FACE ( 'NONE', ( #5862 ), #14217, .F. ) ;
#6173 = EDGE_LOOP ( 'NONE', ( #2459, #5017, #9780, #6965, #6822, #11090 ) ) ;
#6174 = CARTESIAN_POINT ( 'NONE',  ( 29.35089333861488115, -5.954459450865362768, -8.283357778048664244 ) ) ;
#6175 = CARTESIAN_POINT ( 'NONE',  ( 30.78070346053490880, -6.209293581256383199, -4.705209693361168455 ) ) ;
#6176 = ORIENTED_EDGE ( 'NONE', *, *, #16826, .T. ) ;
#6177 = CARTESIAN_POINT ( 'NONE',  ( 29.91004888286193619, -6.613999042680076990, -4.533357778048668685 ) ) ;
#6178 = CARTESIAN_POINT ( 'NONE',  ( 30.71189515440122975, -6.854751018602581958, -5.783357778048663356 ) ) ;
#6179 = ADVANCED_FACE ( 'NONE', ( #7154 ), #8782, .F. ) ;
#6180 = CARTESIAN_POINT ( 'NONE',  ( 0.000000000000000000, 0.000000000000000000, 0.000000000000000000 ) ) ;
#6181 = AXIS2_PLACEMENT_3D ( 'NONE', #9067, #15870, #4792 ) ;
#6182 = CARTESIAN_POINT ( 'NONE',  ( 26.01652455409633902, -4.902371455920926380, 5.783357778048663356 ) ) ;
#6183 = CARTESIAN_POINT ( 'NONE',  ( 28.76238721243587193, -5.825490297734302381, -3.627061608673667781 ) ) ;
#6184 = FACE_OUTER_BOUND ( 'NONE', #3876, .T. ) ;
#6185 = CARTESIAN_POINT ( 'NONE',  ( 27.50903986916043920, -7.240631829073577386, -6.453230759126468818 ) ) ;
#6186 = CARTESIAN_POINT ( 'NONE',  ( 27.45957062324739084, -6.182326487390971792, 3.283357778048663356 ) ) ;
#6187 = CARTESIAN_POINT ( 'NONE',  ( 27.49335874655903567, -6.905162478240574053, -7.033357778048666908 ) ) ;
#6188 = DIRECTION ( 'NONE',  ( -0.1196152422706610735, 0.9928203230275511881, 0.000000000000000000 ) ) ;
#6189 = CARTESIAN_POINT ( 'NONE',  ( 31.28415083292585663, -5.521667582366822202, 7.939653947423658487 ) ) ;
#6190 = EDGE_CURVE ( 'NONE', #15926, #13835, #12857, .T. ) ;
#6191 = ORIENTED_EDGE ( 'NONE', *, *, #5451, .T. ) ;
#6192 = DIRECTION ( 'NONE',  ( 0.000000000000000000, 0.000000000000000000, 1.000000000000000000 ) ) ;
#6193 = FACE_OUTER_BOUND ( 'NONE', #6396, .T. ) ;
#6194 = DIRECTION ( 'NONE',  ( 1.000000000000000000, 0.000000000000000000, 0.000000000000000000 ) ) ;
#6195 = EDGE_CURVE ( 'NONE', #1319, #7967, #12665, .T. ) ;
#6196 = ORIENTED_EDGE ( 'NONE', *, *, #17524, .F. ) ;
#6197 =( REPRESENTATION_RELATIONSHIP ('NONE','NONE', #3227, #5639 ) REPRESENTATION_RELATIONSHIP_WITH_TRANSFORMATION ( #14100 )SHAPE_REPRESENTATION_RELATIONSHIP( ) );
#6198 = CARTESIAN_POINT ( 'NONE',  ( 26.30098629108390895, -7.263436720211717379, 4.952770188466288026 ) ) ;
#6199 = CARTESIAN_POINT ( 'NONE',  ( 31.66250999073069750, -5.675955295111850596, -3.283357778048667797 ) ) ;
#6200 = DIRECTION ( 'NONE',  ( 0.000000000000000000, 0.000000000000000000, -1.000000000000000000 ) ) ;
#6201 = CARTESIAN_POINT ( 'NONE',  ( -34.91600907648203389, -11.88801210197604341, 11.56671555609732671 ) ) ;
#6202 = VERTEX_POINT ( 'NONE', #13029 ) ;
#6203 = DIRECTION ( 'NONE',  ( 0.000000000000000000, 0.000000000000000000, 1.000000000000000000 ) ) ;
#6204 = EDGE_LOOP ( 'NONE', ( #17925, #15517, #16396, #6373 ) ) ;
#6205 = ADVANCED_FACE ( 'NONE', ( #10214 ), #1809, .T. ) ;
#6206 = CARTESIAN_POINT ( 'NONE',  ( 29.30958546476020743, -4.505622649006972402, -8.283357778048662468 ) ) ;
#6207 = LINE ( 'NONE', #17581, #12163 ) ;
#6208 = CONTEXT_DEPENDENT_SHAPE_REPRESENTATION ( #1021, #5328 ) ;
#6209 = LINE ( 'NONE', #11818, #14162 ) ;
#6210 = EDGE_LOOP ( 'NONE', ( #4849, #12012, #12675, #15454 ) ) ;
#6211 = CARTESIAN_POINT ( 'NONE',  ( 30.18087924896149588, -5.654590020340094725, -3.627061608673668225 ) ) ;
#6212 = LINE ( 'NONE', #16111, #4146 ) ;
#6213 = CARTESIAN_POINT ( 'NONE',  ( 38.68147913031997831, -1.341155523753223555, -2.283357778048670461 ) ) ;
#6214 = CARTESIAN_POINT ( 'NONE',  ( 28.40332666278570173, -4.614808937445885384, 3.627061608673664228 ) ) ;
#6215 = EDGE_CURVE ( 'NONE', #2334, #4359, #17949, .T. ) ;
#6216 = ORIENTED_EDGE ( 'NONE', *, *, #883, .F. ) ;
#6217 = CARTESIAN_POINT ( 'NONE',  ( 26.36761712467744090, -6.740983333149474177, -4.705209693361168455 ) ) ;
#6218 = VECTOR ( 'NONE', #1471, 1000.000000000000000 ) ;
#6219 = ORIENTED_EDGE ( 'NONE', *, *, #1946, .F. ) ;
#6220 = CARTESIAN_POINT ( 'NONE',  ( 25.62757597683262034, -3.695291012717980994, 3.627061608673666893 ) ) ;
#6221 = CARTESIAN_POINT ( 'NONE',  ( -29.25000000000000000, -15.80023397548365871, 13.37255996287876592 ) ) ;
#6222 = CARTESIAN_POINT ( 'NONE',  ( 12.70000000000000284, 1.555301434917138827E-15, 0.000000000000000000 ) ) ;
#6223 = ORIENTED_EDGE ( 'NONE', *, *, #6159, .F. ) ;
#6224 = CARTESIAN_POINT ( 'NONE',  ( 30.35023428074701002, -1.862166024106576057, 5.783357778048662468 ) ) ;
#6225 = VERTEX_POINT ( 'NONE', #4509 ) ;
#6226 = CARTESIAN_POINT ( 'NONE',  ( 26.30941689637695902, -7.333411717640721861, -6.290568369890759293 ) ) ;
#6227 = CARTESIAN_POINT ( 'NONE',  ( 28.09753128235661279, -6.832371619143005503, -4.533357778048668685 ) ) ;
#6228 = EDGE_CURVE ( 'NONE', #11475, #3307, #11385, .T. ) ;
#6229 = STYLED_ITEM ( 'NONE', ( #9045 ), #5711 ) ;
#6230 = CYLINDRICAL_SURFACE ( 'NONE', #248, 2.500000000000001776 ) ;
#6231 = DIRECTION ( 'NONE',  ( 0.6000000000000001998, -0.7999999999999999334, 0.000000000000000000 ) ) ;
#6232 = CARTESIAN_POINT ( 'NONE',  ( 26.35439372113758694, -4.861664893681965083, -7.939653947423662039 ) ) ;
#6233 = CARTESIAN_POINT ( 'NONE',  ( -5.500000000000000888, -20.49999999999999645, -12.00000000000000000 ) ) ;
#6234 = CARTESIAN_POINT ( 'NONE',  ( 33.04340326765378677, -1.875050963503474222, 7.033357778048666020 ) ) ;
#6235 = EDGE_CURVE ( 'NONE', #1570, #2089, #17079, .T. ) ;
#6236 = ADVANCED_FACE ( 'NONE', ( #16759 ), #5767, .T. ) ;
#6237 = ORIENTED_EDGE ( 'NONE', *, *, #14569, .T. ) ;
#6238 = EDGE_LOOP ( 'NONE', ( #5752, #2113, #5133, #5416, #17891 ) ) ;
#6239 = VERTEX_POINT ( 'NONE', #4595 ) ;
#6240 = AXIS2_PLACEMENT_3D ( 'NONE', #15008, #17941, #15274 ) ;
#6241 = CARTESIAN_POINT ( 'NONE',  ( 26.56758885001203652, -2.317900097157796324, 5.783357778048657138 ) ) ;
#6242 = CARTESIAN_POINT ( 'NONE',  ( 32.91278983782564183, -5.325448745358647429, 3.627061608673662896 ) ) ;
#6243 = CARTESIAN_POINT ( 'NONE',  ( 0.000000000000000000, 0.000000000000000000, 12.00000000000000000 ) ) ;
#6244 = CARTESIAN_POINT ( 'NONE',  ( 21.42601376483257880, 2.765314980223224417, -6.000000000000000000 ) ) ;
#6245 = CARTESIAN_POINT ( 'NONE',  ( -25.01192583800304448, -22.13892749297381002, -14.47384481777684151 ) ) ;
#6246 = CARTESIAN_POINT ( 'NONE',  ( 27.63266882139180680, -2.199775856772564708, -5.783357778048658027 ) ) ;
#6247 = CARTESIAN_POINT ( 'NONE',  ( 29.07687923786957285, -2.352938776424351008, 4.533357778048667797 ) ) ;
#6248 = CARTESIAN_POINT ( 'NONE',  ( 27.55969062878875064, -7.234529412811931515, -5.783357778048668685 ) ) ;
#6249 = CARTESIAN_POINT ( 'NONE',  ( 16.03720890403358013, 12.19600435288735341, 16.13737481314213440 ) ) ;
#6250 = CARTESIAN_POINT ( 'NONE',  ( 31.35480929215617252, -6.439933945126671055, -7.033357778048666908 ) ) ;
#6251 = EDGE_CURVE ( 'NONE', #13835, #6811, #7610, .T. ) ;
#6252 = CARTESIAN_POINT ( 'NONE',  ( 21.42418217458643070, -10.16661967303011771, 15.24537580551290183 ) ) ;
#6253 = EDGE_CURVE ( 'NONE', #4537, #5547, #7768, .T. ) ;
#6254 =( LENGTH_UNIT ( ) NAMED_UNIT ( * ) SI_UNIT ( .MILLI., .METRE. ) );
#6255 = ORIENTED_EDGE ( 'NONE', *, *, #1638, .T. ) ;
#6256 = ORIENTED_EDGE ( 'NONE', *, *, #3942, .T. ) ;
#6257 = CARTESIAN_POINT ( 'NONE',  ( 27.61527553138257574, -4.709753535998224550, -7.939653947423662039 ) ) ;
#6258 = CARTESIAN_POINT ( 'NONE',  ( 31.54230778485832332, -2.355712103769039611, -4.705209693361160461 ) ) ;
#6259 = ORIENTED_EDGE ( 'NONE', *, *, #6823, .T. ) ;
#6260 = DIRECTION ( 'NONE',  ( 0.9979201627913403261, -0.06446199418653547619, 0.000000000000000000 ) ) ;
#6261 = CARTESIAN_POINT ( 'NONE',  ( 26.31556265977298992, -7.384422263489805793, -5.783357778048663356 ) ) ;
#6262 = ORIENTED_EDGE ( 'NONE', *, *, #10328, .F. ) ;
#6263 = CARTESIAN_POINT ( 'NONE',  ( -34.91600907648203389, -11.88801210197604341, -12.00000000000000000 ) ) ;
#6264 = CARTESIAN_POINT ( 'NONE',  ( 30.76748005699505129, -4.329975141788874993, -7.939653947423662039 ) ) ;
#6265 = VERTEX_POINT ( 'NONE', #1625 ) ;
#6266 = CARTESIAN_POINT ( 'NONE',  ( 29.11750682573587312, -2.010685337989277954, -5.113484796970851676 ) ) ;
#6267 = CARTESIAN_POINT ( 'NONE',  ( 0.000000000000000000, 0.000000000000000000, -3.000000000000000000 ) ) ;
#6268 = ORIENTED_EDGE ( 'NONE', *, *, #15189, .T. ) ;
#6269 = CARTESIAN_POINT ( 'NONE',  ( 1.746467850512308208E-21, -1.591841644184202181E-21, -6.005572809000082835 ) ) ;
#6270 = CARTESIAN_POINT ( 'NONE',  ( 30.96820195323705605, -2.125071739898741097, -7.033357778048658027 ) ) ;
#6271 = EDGE_CURVE ( 'NONE', #4942, #172, #1739, .T. ) ;
#6272 = ORIENTED_EDGE ( 'NONE', *, *, #710, .F. ) ;
#6273 = EDGE_CURVE ( 'NONE', #761, #1670, #11225, .T. ) ;
#6274 = CARTESIAN_POINT ( 'NONE',  ( 27.30005507882132676, -4.747731375419166788, -3.627061608673664672 ) ) ;
#6275 = CARTESIAN_POINT ( 'NONE',  ( 26.31308423962587995, -7.363851090081254824, -5.799730202602000340 ) ) ;
#6276 = CARTESIAN_POINT ( 'NONE',  ( 27.49335874655903567, -6.905162478240574053, -7.033357778048666908 ) ) ;
#6277 = CARTESIAN_POINT ( 'NONE',  ( 14.00000000000000178, -1.714505518806294835E-15, 8.700000000000001066 ) ) ;
#6278 = CARTESIAN_POINT ( 'NONE',  ( 26.55511561737958814, -2.656761491791831187, -7.033357778048658027 ) ) ;
#6279 = CARTESIAN_POINT ( 'NONE',  ( 31.38469755857769528, -2.374701023479507178, -4.705209693361161349 ) ) ;
#6280 = EDGE_CURVE ( 'NONE', #16733, #4586, #12456, .T. ) ;
#6281 = ORIENTED_EDGE ( 'NONE', *, *, #12115, .F. ) ;
#6282 = CARTESIAN_POINT ( 'NONE',  ( 30.71189515440122975, -6.854751018602581958, -5.783357778048663356 ) ) ;
#6283 = FACE_OUTER_BOUND ( 'NONE', #4542, .T. ) ;
#6284 = DIRECTION ( 'NONE',  ( 0.000000000000000000, 0.000000000000000000, 1.000000000000000000 ) ) ;
#6285 = ORIENTED_EDGE ( 'NONE', *, *, #4199, .F. ) ;
#6286 = CARTESIAN_POINT ( 'NONE',  ( -5.500000000000000888, -20.49999999999999645, 13.00000000000000178 ) ) ;
#6287 = CARTESIAN_POINT ( 'NONE',  ( 31.43732351782677625, -4.249272233123119413, -3.283357778048664688 ) ) ;
#6288 = CARTESIAN_POINT ( 'NONE',  ( 15.92260893619738837, -28.39189527176317540, 0.000000000000000000 ) ) ;
#6289 = AXIS2_PLACEMENT_3D ( 'NONE', #1124, #8101, #16716 ) ;
#6290 = CARTESIAN_POINT ( 'NONE',  ( -12.50000000000000000, 0.000000000000000000, -12.00000000000000000 ) ) ;
#6291 = ORIENTED_EDGE ( 'NONE', *, *, #10457, .F. ) ;
#6292 = CARTESIAN_POINT ( 'NONE',  ( 30.09392748191118017, -6.591845302810410701, 4.533357778048659803 ) ) ;
#6293 = EDGE_CURVE ( 'NONE', #2108, #11560, #10947, .T. ) ;
#6294 = CARTESIAN_POINT ( 'NONE',  ( 30.75815651034531584, -7.238725614818142695, -5.783357778048669573 ) ) ;
#6295 = DIRECTION ( 'NONE',  ( -0.1196152422706621143, -0.9928203230275509661, -0.000000000000000000 ) ) ;
#6296 = CONTEXT_DEPENDENT_SHAPE_REPRESENTATION ( #4473, #1011 ) ;
#6297 = DIRECTION ( 'NONE',  ( 0.000000000000000000, 1.000000000000000000, 0.000000000000000000 ) ) ;
#6298 = DIRECTION ( 'NONE',  ( 0.9928203230275512992, 0.1196152422706610180, 4.006172263299093133E-17 ) ) ;
#6299 = CARTESIAN_POINT ( 'NONE',  ( 30.39102621733566423, -5.629271460726126719, -7.939653947423664704 ) ) ;
#6300 = CARTESIAN_POINT ( 'NONE',  ( 45.50000000000000000, -19.03270077640483038, 5.537981825772250843 ) ) ;
#6301 = CARTESIAN_POINT ( 'NONE',  ( 25.76466184735054910, -2.811881907026620553, -6.248149982130924762 ) ) ;
#6302 = CARTESIAN_POINT ( 'NONE',  ( 33.59503905791412137, -1.808589744724287129, 7.033357778048666020 ) ) ;
#6303 = EDGE_CURVE ( 'NONE', #9649, #3432, #10695, .T. ) ;
#6304 = AXIS2_PLACEMENT_3D ( 'NONE', #11715, #15812, #6192 ) ;
#6305 = ORIENTED_EDGE ( 'NONE', *, *, #5084, .F. ) ;
#6306 = CARTESIAN_POINT ( 'NONE',  ( 26.30054492745255246, -7.259773351106303174, 6.331581338229590017 ) ) ;
#6307 = ORIENTED_EDGE ( 'NONE', *, *, #17118, .F. ) ;
#6308 = CARTESIAN_POINT ( 'NONE',  ( 32.93018312783485158, -2.815471066132994249, 7.939653947423664704 ) ) ;
#6309 = CARTESIAN_POINT ( 'NONE',  ( 26.01652455409633902, -4.902371455920928156, -5.783357778048663356 ) ) ;
#6310 = EDGE_LOOP ( 'NONE', ( #10088, #13409, #13253, #6086, #11876, #12705, #6860 ) ) ;
#6311 = DIRECTION ( 'NONE',  ( -0.000000000000000000, -0.000000000000000000, -1.000000000000000000 ) ) ;
#6312 = VERTEX_POINT ( 'NONE', #10807 ) ;
#6313 = CARTESIAN_POINT ( 'NONE',  ( -9.500000000000000000, 0.000000000000000000, 1.102182119232619020E-16 ) ) ;
#6314 = LINE ( 'NONE', #10384, #17185 ) ;
#6315 = DIRECTION ( 'NONE',  ( -0.000000000000000000, 0.8660254037844391517, 0.4999999999999991673 ) ) ;
#6316 = CARTESIAN_POINT ( 'NONE',  ( 32.64557936882268052, -2.222789665795767089, -4.705209693361161349 ) ) ;
#6317 = AXIS2_PLACEMENT_3D ( 'NONE', #9059, #7523, #11678 ) ;
#6318 = CARTESIAN_POINT ( 'NONE',  ( -0.5469803261936758698, 4.303002914946057800, -3.235259548912099881 ) ) ;
#6319 = AXIS2_PLACEMENT_3D ( 'NONE', #5569, #2860, #5658 ) ;
#6320 = CARTESIAN_POINT ( 'NONE',  ( -31.74999999999995737, 3.061616997868383634E-16, -2.500000000000000444 ) ) ;
#6321 = CARTESIAN_POINT ( 'NONE',  ( 28.10549950023366961, -2.142809097641162897, -5.783357778048658027 ) ) ;
#6322 = DIRECTION ( 'NONE',  ( -0.9928203230275512992, -0.1196152422706610180, -4.006172263299093133E-17 ) ) ;
#6323 = CARTESIAN_POINT ( 'NONE',  ( 31.51612863268893960, -4.239777773060436239, 8.283357778048662468 ) ) ;
#6324 = VERTEX_POINT ( 'NONE', #9460 ) ;
#6325 = ORIENTED_EDGE ( 'NONE', *, *, #3962, .T. ) ;
#6326 = ORIENTED_EDGE ( 'NONE', *, *, #9588, .F. ) ;
#6327 = AXIS2_PLACEMENT_3D ( 'NONE', #5225, #16404, #3886 ) ;
#6328 = VERTEX_POINT ( 'NONE', #15091 ) ;
#6329 = EDGE_CURVE ( 'NONE', #11222, #6357, #1510, .T. ) ;
#6330 = CARTESIAN_POINT ( 'NONE',  ( 26.23609683341064525, -2.995005734021441768, 4.705209693361167567 ) ) ;
#6331 =( REPRESENTATION_RELATIONSHIP ('NONE','NONE', #3227, #12009 ) REPRESENTATION_RELATIONSHIP_WITH_TRANSFORMATION ( #3590 )SHAPE_REPRESENTATION_RELATIONSHIP( ) );
#6332 = CARTESIAN_POINT ( 'NONE',  ( 33.54323074294813267, -5.249493066516778050, 3.627061608673662896 ) ) ;
#6333 = ORIENTED_EDGE ( 'NONE', *, *, #1569, .T. ) ;
#6334 = CARTESIAN_POINT ( 'NONE',  ( 29.18947247604338102, -3.066280307211263434, -8.283357778048660691 ) ) ;
#6335 = CARTESIAN_POINT ( 'NONE',  ( -27.11285657029384666, -20.94160726625447211, -13.95434672273383114 ) ) ;
#6336 = CARTESIAN_POINT ( 'NONE',  ( 29.13014440709066832, -5.781182818409868140, -7.939653947423664704 ) ) ;
#6337 = CARTESIAN_POINT ( 'NONE',  ( 29.35089333861488115, -5.954459450865362768, 3.283357778048663356 ) ) ;
#6338 = CARTESIAN_POINT ( 'NONE',  ( 32.83754810739939956, -9.116730809865838836, -5.783357778048662468 ) ) ;
#6339 = AXIS2_PLACEMENT_3D ( 'NONE', #15041, #9581, #6611 ) ;
#6340 = CARTESIAN_POINT ( 'NONE',  ( 32.64947922571280259, -7.010858578292532783, -5.783357778048669573 ) ) ;
#6341 = CARTESIAN_POINT ( 'NONE',  ( -2.749999999999988454, -20.49999999999999645, 13.00000000000000355 ) ) ;
#6342 = CARTESIAN_POINT ( 'NONE',  ( 29.69163902039066372, -1.941513746749485847, -6.453230759126468818 ) ) ;
#6343 = PRESENTATION_STYLE_ASSIGNMENT (( #6528 ) ) ;
#6344 = AXIS2_PLACEMENT_3D ( 'NONE', #16491, #5588, #16673 ) ;
#6345 = CARTESIAN_POINT ( 'NONE',  ( 28.14933959732260149, -3.391468297350501260, -7.939653947423660263 ) ) ;
#6346 = CARTESIAN_POINT ( 'NONE',  ( 32.18597209352066812, -4.159074864394664672, -7.939653947423662039 ) ) ;
#6347 = EDGE_LOOP ( 'NONE', ( #1795, #7350, #16181, #3014, #9027, #402 ) ) ;
#6348 = CARTESIAN_POINT ( 'NONE',  ( 4.000000000000000000, -2.309401076758510918, -3.133295621305383083 ) ) ;
#6349 = CARTESIAN_POINT ( 'NONE',  ( -7.374038404635891553, 5.989453865500174778, -2.000000000000000000 ) ) ;
#6350 = AXIS2_PLACEMENT_3D ( 'NONE', #14400, #16953, #15395 ) ;
#6351 = AXIS2_PLACEMENT_3D ( 'NONE', #14293, #7748, #2235 ) ;
#6352 = PRODUCT ( 'Bleed Screw Nipple', 'Bleed Screw Nipple', '', ( #12559 ) ) ;
#6353 =( BOUNDED_CURVE ( )  B_SPLINE_CURVE ( 3, ( #10109, #10208, #15755, #10290 ),
 .UNSPECIFIED., .F., .T. ) 
 B_SPLINE_CURVE_WITH_KNOTS ( ( 4, 4 ),
 ( 0.000000000000000000, 3.141592653589793116 ),
 .UNSPECIFIED. ) 
 CURVE ( )  GEOMETRIC_REPRESENTATION_ITEM ( )  RATIONAL_B_SPLINE_CURVE ( ( 1.000000000000000000, 0.3333333333333333703, 0.3333333333333333703, 1.000000000000000000 ) ) 
 REPRESENTATION_ITEM ( '' )  );
#6354 = ORIENTED_EDGE ( 'NONE', *, *, #12904, .T. ) ;
#6355 = EDGE_CURVE ( 'NONE', #5547, #4193, #7218, .T. ) ;
#6356 = CARTESIAN_POINT ( 'NONE',  ( 31.51621784984448738, -6.120678622607529817, -6.861505862736166250 ) ) ;
#6357 = VERTEX_POINT ( 'NONE', #6835 ) ;
#6358 = DIRECTION ( 'NONE',  ( -0.000000000000000000, -0.000000000000000000, -1.000000000000000000 ) ) ;
#6359 = CARTESIAN_POINT ( 'NONE',  ( 33.64386668575551198, -3.983427357176565486, -8.283357778048662468 ) ) ;
#6360 = CARTESIAN_POINT ( 'NONE',  ( -35.46635924378174565, -16.45598204045937152, -11.37070560279562059 ) ) ;
#6361 = CARTESIAN_POINT ( 'NONE',  ( -3.999999999999999112, 1.539600717838999877, -3.000726591567080881 ) ) ;
#6362 = CARTESIAN_POINT ( 'NONE',  ( 32.29295089585319545, -5.599999616269980329, -3.283357778048667797 ) ) ;
#6363 = VECTOR ( 'NONE', #2593, 1000.000000000000114 ) ;
#6364 = VECTOR ( 'NONE', #2304, 1000.000000000000227 ) ;
#6365 = CARTESIAN_POINT ( 'NONE',  ( 26.36761712467744090, -6.740983333149474177, -4.705209693361168455 ) ) ;
#6366 = CARTESIAN_POINT ( 'NONE',  ( 25.90934487712385348, 0.1208734971681838660, -5.783357778048663356 ) ) ;
#6367 = CARTESIAN_POINT ( 'NONE',  ( 30.37154917142620292, -2.923863409590206519, -8.283357778048660691 ) ) ;
#6368 = CARTESIAN_POINT ( 'NONE',  ( 4.235887314095728939, 2.417314327725964773, -3.451162025751985496 ) ) ;
#6369 = CARTESIAN_POINT ( 'NONE',  ( 28.01872616749444944, -6.841866079205687790, -4.533357778048668685 ) ) ;
#6370 = AXIS2_PLACEMENT_3D ( 'NONE', #11468, #14309, #4325 ) ;
#6371 = CARTESIAN_POINT ( 'NONE',  ( 33.28924367748503244, -4.026152426421394814, -7.939653947423662039 ) ) ;
#6372 = EDGE_CURVE ( 'NONE', #4560, #14000, #17679, .T. ) ;
#6373 = ORIENTED_EDGE ( 'NONE', *, *, #10552, .T. ) ;
#6374 = PLANE ( 'NONE',  #4843 ) ;
#6375 = B_SPLINE_CURVE_WITH_KNOTS ( 'NONE', 3,
 ( #15245, #1655, #9610, #1472 ),
 .UNSPECIFIED., .F., .F.,
 ( 4, 4 ),
 ( 0.007932485430080135971, 0.009354825709699440481 ),
 .UNSPECIFIED. ) ;
#6376 = CARTESIAN_POINT ( 'NONE',  ( 26.63392073224175505, -2.647267031729148012, -7.033357778048658027 ) ) ;
#6377 = CARTESIAN_POINT ( 'NONE',  ( -1.828356344711642878, -3.563200125723190670, -8.309957901196191823E-15 ) ) ;
#6378 = ORIENTED_EDGE ( 'NONE', *, *, #6, .F. ) ;
#6379 = CARTESIAN_POINT ( 'NONE',  ( 33.95908713831674675, -3.945449517755637903, 5.783357778048663356 ) ) ;
#6381 = ORIENTED_EDGE ( 'NONE', *, *, #7718, .F. ) ;
#6380 = PLANE ( 'NONE',  #11317 ) ;
#6382 = VECTOR ( 'NONE', #743, 1000.000000000000000 ) ;
#6383 = FACE_OUTER_BOUND ( 'NONE', #3190, .T. ) ;
#6384 = CARTESIAN_POINT ( 'NONE',  ( 29.79859849048667897, -1.928627242885762705, 5.783357778048662468 ) ) ;
#6385 = EDGE_CURVE ( 'NONE', #825, #16104, #13813, .T. ) ;
#6386 = CARTESIAN_POINT ( 'NONE',  ( 28.04870365451522218, -4.657534006690712935, -8.283357778048662468 ) ) ;
#6387 = DIRECTION ( 'NONE',  ( 0.7999999999999999334, -0.6000000000000001998, 0.000000000000000000 ) ) ;
#6388 = AXIS2_PLACEMENT_3D ( 'NONE', #13116, #10632, #11655 ) ;
#6389 = ITEM_DEFINED_TRANSFORMATION ( 'NONE', 'NONE', #14895,  #3575 ) ;
#6390 = FACE_OUTER_BOUND ( 'NONE', #11076, .T. ) ;
#6391 = CYLINDRICAL_SURFACE ( 'NONE', #15852, 2.500000000000001776 ) ;
#6392 = B_SPLINE_CURVE_WITH_KNOTS ( 'NONE', 3,
 ( #3775, #3684, #9299, #4765 ),
 .UNSPECIFIED., .F., .F.,
 ( 4, 4 ),
 ( 0.007932485430080137706, 0.009354825709699442216 ),
 .UNSPECIFIED. ) ;
#6393 = CARTESIAN_POINT ( 'NONE',  ( 30.41294626588012306, -6.253601060580800564, -6.861505862736167138 ) ) ;
#6394 = DIRECTION ( 'NONE',  ( 1.000000000000000000, 0.000000000000000000, 0.000000000000000000 ) ) ;
#6395 = CARTESIAN_POINT ( 'NONE',  ( 27.02867472334902033, -6.034368414549446058, 7.939653947423658487 ) ) ;
#6396 = EDGE_LOOP ( 'NONE', ( #7632, #1696, #7456, #17026 ) ) ;
#6397 = AXIS2_PLACEMENT_3D ( 'NONE', #14054, #12684, #9681 ) ;
#6398 = ORIENTED_EDGE ( 'NONE', *, *, #11670, .F. ) ;
#6399 = ADVANCED_FACE ( 'NONE', ( #1588 ), #3118, .T. ) ;
#6400 = ORIENTED_EDGE ( 'NONE', *, *, #5443, .T. ) ;
#6401 = CARTESIAN_POINT ( 'NONE',  ( 28.93739072872572393, -3.296523698798161650, 3.627061608673666893 ) ) ;
#6402 = CARTESIAN_POINT ( 'NONE',  ( -25.76257153370368869, -10.59741316493651730, 14.29454127969954591 ) ) ;
#6403 = CARTESIAN_POINT ( 'NONE',  ( 27.48088551392658729, -7.244023872874614689, -5.783357778048657138 ) ) ;
#6404 = AXIS2_PLACEMENT_3D ( 'NONE', #12619, #199, #11227 ) ;
#6405 = ORIENTED_EDGE ( 'NONE', *, *, #738, .F. ) ;
#6406 = AXIS2_PLACEMENT_3D ( 'NONE', #3295, #11518, #16910 ) ;
#6407 = DIRECTION ( 'NONE',  ( -0.000000000000000000, -0.000000000000000000, 1.000000000000000000 ) ) ;
#6408 = CARTESIAN_POINT ( 'NONE',  ( 39.19942832275109623, -5.640193629429882449, -1.783357778048662690 ) ) ;
#6409 = DIRECTION ( 'NONE',  ( -0.9928203230275512992, -0.1196152422706610180, -4.006172263299093133E-17 ) ) ;
#6410 = CARTESIAN_POINT ( 'NONE',  ( 32.08959525433819238, -2.916745304588811649, -7.939653947423660263 ) ) ;
#6411 = EDGE_CURVE ( 'NONE', #11056, #3273, #7030, .T. ) ;
#6412 = VECTOR ( 'NONE', #7305, 999.9999999999998863 ) ;
#6413 = CARTESIAN_POINT ( 'NONE',  ( 31.08270050955629671, -4.291997302367946077, -3.627061608673664672 ) ) ;
#6414 = CARTESIAN_POINT ( 'NONE',  ( 28.60033944477555323, -4.591072787911525843, -8.283357778048662468 ) ) ;
#6415 = CARTESIAN_POINT ( 'NONE',  ( -2.016448651773435938E-27, -20.49999999999999645, -13.00000000000000178 ) ) ;
#6416 = CARTESIAN_POINT ( 'NONE',  ( 28.38593337277646711, -7.124786616671554107, -5.783357778048668685 ) ) ;
#6417 = CARTESIAN_POINT ( 'NONE',  ( 36.27615609941022257, -23.17738945083361557, 0.000000000000000000 ) ) ;
#6418 = CARTESIAN_POINT ( 'NONE',  ( 27.73348320195396965, -4.695511846111656062, -3.283357778048664688 ) ) ;
#6419 = FACE_OUTER_BOUND ( 'NONE', #3643, .T. ) ;
#6420 = STYLED_ITEM ( 'NONE', ( #5437 ), #11123 ) ;
#6421 = CARTESIAN_POINT ( 'NONE',  ( 26.90793483298706690, -6.248787706170159773, 3.283357778048663800 ) ) ;
#6422 = EDGE_LOOP ( 'NONE', ( #14409, #6519, #3906, #10325, #6714 ) ) ;
#6423 = VERTEX_POINT ( 'NONE', #11154 ) ;
#6424 = VECTOR ( 'NONE', #4084, 1000.000000000000227 ) ;
#6425 = EDGE_CURVE ( 'NONE', #3366, #10034, #7395, .T. ) ;
#6426 = EDGE_LOOP ( 'NONE', ( #15768, #866, #6943, #14731 ) ) ;
#6427 = CARTESIAN_POINT ( 'NONE',  ( 26.66961417369883591, -4.823687054261037055, 7.939653947423662039 ) ) ;
#6428 = CARTESIAN_POINT ( 'NONE',  ( 7.499998387031003411, -20.49508120620799900, 17.00000000000000000 ) ) ;
#6429 = ORIENTED_EDGE ( 'NONE', *, *, #16598, .F. ) ;
#6430 = SURFACE_STYLE_FILL_AREA ( #15958 ) ;
#6431 = CARTESIAN_POINT ( 'NONE',  ( 38.64694918415791136, -1.054552983374777098, -1.783357778048662912 ) ) ;
#6432 = CARTESIAN_POINT ( 'NONE',  ( 27.48088551392658729, -7.244023872874614689, -5.783357778048657138 ) ) ;
#6433 = CARTESIAN_POINT ( 'NONE',  ( 31.06530721954707985, -6.801974981593605030, -5.783357778048669573 ) ) ;
#6434 = CARTESIAN_POINT ( 'NONE',  ( 31.35480929215617252, -6.439933945126671055, -7.033357778048666908 ) ) ;
#6436 = EDGE_CURVE ( 'NONE', #6324, #2403, #1866, .T. ) ;
#6435 = CARTESIAN_POINT ( 'NONE',  ( 1.499999999999999334, -5.809475019311126864, -2.000000000000000000 ) ) ;
#6437 = CARTESIAN_POINT ( 'NONE',  ( 32.93832978346670615, -1.887710243310447567, -7.033357778048658027 ) ) ;
#6438 = DIRECTION ( 'NONE',  ( -0.000000000000000000, -0.000000000000000000, -1.000000000000000000 ) ) ;
#6439 = CARTESIAN_POINT ( 'NONE',  ( 25.78518620311324838, -3.676302093007511651, -7.939653947423660263 ) ) ;
#6440 = CARTESIAN_POINT ( 'NONE',  ( 17.59269349951685157, -13.05689734314391970, 15.91118832497637570 ) ) ;
#6441 = CIRCLE ( 'NONE', #10757, 2.500000000000000000 ) ;
#6442 = AXIS2_PLACEMENT_3D ( 'NONE', #2305, #750, #7996 ) ;
#6443 = EDGE_CURVE ( 'NONE', #8696, #1570, #5643, .T. ) ;
#6444 = CARTESIAN_POINT ( 'NONE',  ( 32.67619606237177265, -1.592130426037603907, -5.783357778048658027 ) ) ;
#6445 = CARTESIAN_POINT ( 'NONE',  ( 31.06530721954707985, -6.801974981593605918, -5.783357778048669573 ) ) ;
#6446 = VERTEX_POINT ( 'NONE', #15263 ) ;
#6447 =( BOUNDED_CURVE ( )  B_SPLINE_CURVE ( 2, ( #1426, #3799, #5138, #8046, #6685, #13584, #1166, #5314, #12219 ),
 .UNSPECIFIED., .F., .T. ) 
 B_SPLINE_CURVE_WITH_KNOTS ( ( 3, 2, 2, 2, 3 ),
 ( 0.3653846153846154188, 0.3717948717948718063, 0.3846153846153846367, 0.3974358974358974117, 0.4038461538461538547 ),
 .UNSPECIFIED. ) 
 CURVE ( )  GEOMETRIC_REPRESENTATION_ITEM ( )  RATIONAL_B_SPLINE_CURVE ( ( 0.9330127018922194093, 0.9330127018922196314, 1.000000000000000000, 0.8660254037844387076, 1.000000000000000000, 0.8660254037844387076, 1.000000000000000000, 0.9330127018922190762, 0.9330127018922194093 ) ) 
 REPRESENTATION_ITEM ( '' )  );
#6448 = CARTESIAN_POINT ( 'NONE',  ( 38.37070961486131182, 1.238267339652773913, -5.783357778048661579 ) ) ;
#6449 = DIRECTION ( 'NONE',  ( -1.000000000000000000, 0.000000000000000000, 0.000000000000000000 ) ) ;
#6450 = EDGE_CURVE ( 'NONE', #512, #8562, #8749, .T. ) ;
#6451 = ORIENTED_EDGE ( 'NONE', *, *, #3385, .T. ) ;
#6452 = CARTESIAN_POINT ( 'NONE',  ( 26.01652455409633902, -4.902371455920926380, 5.783357778048663356 ) ) ;
#6453 = AXIS2_PLACEMENT_3D ( 'NONE', #136, #2590, #2501 ) ;
#6454 = CARTESIAN_POINT ( 'NONE',  ( 33.30246708102489350, -5.905470865888903020, -4.705209693361168455 ) ) ;
#6455 = ORIENTED_EDGE ( 'NONE', *, *, #15879, .F. ) ;
#6456 = CIRCLE ( 'NONE', #14271, 10.50000000000000000 ) ;
#6457 = CARTESIAN_POINT ( 'NONE',  ( 10.37836969302994028, -0.6704047395399680420, -6.899999999999998579 ) ) ;
#6458 = LINE ( 'NONE', #742, #1816 ) ;
#6459 = CARTESIAN_POINT ( 'NONE',  ( 25.83973938098743162, -3.435034105423888207, 7.359589145280891032 ) ) ;
#6460 = DIRECTION ( 'NONE',  ( 0.000000000000000000, 0.000000000000000000, 1.000000000000000000 ) ) ;
#6461 = CARTESIAN_POINT ( 'NONE',  ( 30.58169613980036772, -2.898544849976259385, -3.283357778048662023 ) ) ;
#6462 = ORIENTED_EDGE ( 'NONE', *, *, #2462, .T. ) ;
#6463 = AXIS2_PLACEMENT_3D ( 'NONE', #17200, #3120, #15816 ) ;
#6464 = EDGE_CURVE ( 'NONE', #6423, #6659, #3208, .T. ) ;
#6465 = DIRECTION ( 'NONE',  ( 1.000000000000000000, 0.000000000000000000, 0.000000000000000000 ) ) ;
#6466 = AXIS2_PLACEMENT_3D ( 'NONE', #16364, #8090, #4009 ) ;
#6467 = LINE ( 'NONE', #6628, #12208 ) ;
#6468 = FACE_BOUND ( 'NONE', #12862, .T. ) ;
#6469 = CARTESIAN_POINT ( 'NONE',  ( 17.88061427385022739, 10.54987872837076601, -15.87467694953868502 ) ) ;
#6470 = ORIENTED_EDGE ( 'NONE', *, *, #11504, .T. ) ;
#6471 = CARTESIAN_POINT ( 'NONE',  ( 28.44643833274707845, -2.428894455266221275, -7.033357778048658027 ) ) ;
#6472 = CARTESIAN_POINT ( 'NONE',  ( 31.93198502805756789, -2.935734224299280548, -7.939653947423660263 ) ) ;
#6473 = ORIENTED_EDGE ( 'NONE', *, *, #1159, .T. ) ;
#6474 = AXIS2_PLACEMENT_3D ( 'NONE', #16581, #5410, #4066 ) ;
#6475 = ADVANCED_FACE ( 'NONE', ( #16726, #16920 ), #11439, .T. ) ;
#6476 = ORIENTED_EDGE ( 'NONE', *, *, #16868, .F. ) ;
#6477 = CARTESIAN_POINT ( 'NONE',  ( 30.42903939560917337, -1.852671564043892660, 5.783357778048667797 ) ) ;
#6478 = CARTESIAN_POINT ( 'NONE',  ( 26.90793483298705979, -6.248787706170159773, -8.283357778048664244 ) ) ;
#6479 = VERTEX_POINT ( 'NONE', #9807 ) ;
#6480 = CARTESIAN_POINT ( 'NONE',  ( 0.000000000000000000, 0.000000000000000000, 10.50000000000000000 ) ) ;
#6481 = DIRECTION ( 'NONE',  ( 1.000000000000000000, 0.000000000000000000, 0.000000000000000000 ) ) ;
#6482 = CARTESIAN_POINT ( 'NONE',  ( -9.166200962222356807, -3.560057785416302689, -2.333128398347827481 ) ) ;
#6483 = EDGE_CURVE ( 'NONE', #2940, #11624, #8279, .T. ) ;
#6484 = CARTESIAN_POINT ( 'NONE',  ( 29.21955148510287614, -5.970283550416647600, -3.283357778048667797 ) ) ;
#6485 = CARTESIAN_POINT ( 'NONE',  ( -3.347071143357316814, -15.22052928361022950, -17.00000000000000000 ) ) ;
#6486 = CONTEXT_DEPENDENT_SHAPE_REPRESENTATION ( #8191, #3751 ) ;
#6487 = CYLINDRICAL_SURFACE ( 'NONE', #2863, 95.00000000000000000 ) ;
#6488 = CARTESIAN_POINT ( 'NONE',  ( -3.538288549924106796, -15.34800872113743431, -13.00000000000000178 ) ) ;
#6489 = CARTESIAN_POINT ( 'NONE',  ( 28.26310972651430120, -2.123820177930694442, -5.783357778048658027 ) ) ;
#6490 = CARTESIAN_POINT ( 'NONE',  ( 32.97402322492378346, -4.064130265842336165, -3.627061608673664672 ) ) ;
#6491 = CARTESIAN_POINT ( 'NONE',  ( 32.93004296264515318, -25.68697430340742471, 12.29384923381407546 ) ) ;
#6492 = CARTESIAN_POINT ( 'NONE',  ( 27.75966235412334981, -2.811446176820259879, 6.861505862736166250 ) ) ;
#6493 = ORIENTED_EDGE ( 'NONE', *, *, #4285, .F. ) ;
#6494 = CARTESIAN_POINT ( 'NONE',  ( 30.82871344409320713, -3.068656662272551738, 3.627061608673666893 ) ) ;
#6495 = CARTESIAN_POINT ( 'NONE',  ( -27.94356719068602146, -12.38857420186734970, 13.73436385264702153 ) ) ;
#6496 = CARTESIAN_POINT ( 'NONE',  ( 5.560781378645573980, 6.809993116116507654E-16, -3.700000000000000178 ) ) ;
#6497 = VERTEX_POINT ( 'NONE', #1770 ) ;
#6498 = SURFACE_SIDE_STYLE ('',( #2340 ) ) ;
#6499 = FACE_OUTER_BOUND ( 'NONE', #6422, .T. ) ;
#6500 = CARTESIAN_POINT ( 'NONE',  ( 7.499998387031003411, -20.49508120620799900, -6.000000000000000000 ) ) ;
#6501 = CARTESIAN_POINT ( 'NONE',  ( 32.67619606237177265, -1.592130426037603907, -5.783357778048658027 ) ) ;
#6502 = CARTESIAN_POINT ( 'NONE',  ( 31.91006497951310550, -2.311404624444611589, -6.861505862736159145 ) ) ;
#6503 = CARTESIAN_POINT ( 'NONE',  ( 28.76992167940542799, -7.088720471389836852, -6.453230759126468818 ) ) ;
#6504 = PLANE ( 'NONE',  #9804 ) ;
#6505 =( NAMED_UNIT ( * ) PLANE_ANGLE_UNIT ( ) SI_UNIT ( $, .RADIAN. ) );
#6506 = CARTESIAN_POINT ( 'NONE',  ( 27.09860475545177039, -3.518061095420291995, 7.939653947423664704 ) ) ;
#6507 = PRODUCT_DEFINITION_SHAPE ( 'NONE', 'NONE',  #17968 ) ;
#6508 = ORIENTED_EDGE ( 'NONE', *, *, #14965, .F. ) ;
#6509 = ADVANCED_FACE ( 'NONE', ( #16821 ), #1495, .F. ) ;
#6510 = CARTESIAN_POINT ( 'NONE',  ( -2.016448651773435938E-27, -20.49999999999999645, -12.00000000000000000 ) ) ;
#6511 = CARTESIAN_POINT ( 'NONE',  ( -8.632250723006720250, -18.84644399697197770, -13.00000000000000178 ) ) ;
#6512 = CARTESIAN_POINT ( 'NONE',  ( 26.16860980394290337, -3.430234601869349920, -3.283357778048662023 ) ) ;
#6513 = CARTESIAN_POINT ( 'NONE',  ( 27.73348320195396965, -4.695511846111656062, 8.283357778048662468 ) ) ;
#6514 = EDGE_LOOP ( 'NONE', ( #15404, #9325, #16717, #7233 ) ) ;
#6515 = ADVANCED_FACE ( 'NONE', ( #7299 ), #14005, .T. ) ;
#6516 = ORIENTED_EDGE ( 'NONE', *, *, #10213, .T. ) ;
#6517 = CARTESIAN_POINT ( 'NONE',  ( 32.56242593318007295, -2.859778545457410281, 3.627061608673666893 ) ) ;
#6518 = CARTESIAN_POINT ( 'NONE',  ( 30.81132015408399027, -5.578634341498224458, 7.939653947423658487 ) ) ;
#6519 = ORIENTED_EDGE ( 'NONE', *, *, #15803, .F. ) ;
#6520 = SURFACE_STYLE_FILL_AREA ( #10307 ) ;
#6521 = DIRECTION ( 'NONE',  ( 0.000000000000000000, 1.000000000000000000, -0.000000000000000000 ) ) ;
#6522 = DIRECTION ( 'NONE',  ( 0.1195020427801297691, -0.9918807541847894926, -0.04349518650597276187 ) ) ;
#6523 = CARTESIAN_POINT ( 'NONE',  ( 29.97942892559193950, -4.424919740341219487, -3.627061608673664672 ) ) ;
#6524 = CARTESIAN_POINT ( 'NONE',  ( 30.40162818048570514, -5.827866652795590241, 8.283357778048660691 ) ) ;
#6525 = DIRECTION ( 'NONE',  ( 0.000000000000000000, 0.000000000000000000, -1.000000000000000000 ) ) ;
#6526 = CARTESIAN_POINT ( 'NONE',  ( 26.31556265977298992, -7.384422263489805793, -5.783357778048663356 ) ) ;
#6527 = CARTESIAN_POINT ( 'NONE',  ( 26.51200394741821498, -4.842675973971495296, -7.939653947423662039 ) ) ;
#6528 = SURFACE_STYLE_USAGE ( .BOTH. , #12043 ) ;
#6529 = EDGE_CURVE ( 'NONE', #10739, #13209, #5255, .T. ) ;
#6530 = CARTESIAN_POINT ( 'NONE',  ( 31.65190802758064592, -5.477360103042387074, -7.939653947423664704 ) ) ;
#6531 = CARTESIAN_POINT ( 'NONE',  ( 31.24031073583692475, -4.273008382657478954, -3.627061608673664672 ) ) ;
#6532 = ORIENTED_EDGE ( 'NONE', *, *, #1518, .F. ) ;
#6533 = DIRECTION ( 'NONE',  ( 0.9928203230275512992, 0.1196152422706614898, -0.000000000000000000 ) ) ;
#6534 = CARTESIAN_POINT ( 'NONE',  ( 26.01652455409633902, -4.902371455920936150, -5.783357778048664244 ) ) ;
#6535 = AXIS2_PLACEMENT_3D ( 'NONE', #2855, #8295, #1244 ) ;
#6536 = EDGE_CURVE ( 'NONE', #17313, #11147, #1190, .T. ) ;
#6537 = VERTEX_POINT ( 'NONE', #13093 ) ;
#6538 = CARTESIAN_POINT ( 'NONE',  ( 33.40754056521197413, -5.892811586081919906, 4.705209693361160461 ) ) ;
#6539 = CARTESIAN_POINT ( 'NONE',  ( 27.71165237056504793, -5.952083095804076684, -7.939653947423662927 ) ) ;
#6540 = DIRECTION ( 'NONE',  ( 0.000000000000000000, 0.000000000000000000, 1.000000000000000000 ) ) ;
#6541 = DIRECTION ( 'NONE',  ( 0.3830490080632377725, -0.9237280213470682178, 0.000000000000000000 ) ) ;
#6542 = FACE_OUTER_BOUND ( 'NONE', #13460, .T. ) ;
#6543 = CARTESIAN_POINT ( 'NONE',  ( 30.61177514885987350, -5.802548093181622235, -8.283357778048662468 ) ) ;
#6544 = ORIENTED_EDGE ( 'NONE', *, *, #7732, .F. ) ;
#6545 = CARTESIAN_POINT ( 'NONE',  ( 0.000000000000000000, 0.000000000000000000, 0.000000000000000000 ) ) ;
#6546 = DIRECTION ( 'NONE',  ( -0.000000000000000000, -0.000000000000000000, -1.000000000000000000 ) ) ;
#6547 = CYLINDRICAL_SURFACE ( 'NONE', #3676, 2.749999999999992006 ) ;
#6548 = CARTESIAN_POINT ( 'NONE',  ( 30.98067518586950442, -1.786210345264705790, -5.783357778048658027 ) ) ;
#6549 = CARTESIAN_POINT ( 'NONE',  ( -2.836862643238851511, -3.208966885971353822, -3.205052026701894707 ) ) ;
#6550 = CARTESIAN_POINT ( 'NONE',  ( 32.34358231980129261, -4.140085944684206432, -3.627061608673664672 ) ) ;
#6551 = EDGE_CURVE ( 'NONE', #14662, #17553, #9511, .T. ) ;
#6552 = CARTESIAN_POINT ( 'NONE',  ( 5.500000000000000888, -20.49999999999999645, -12.00000000000000000 ) ) ;
#6553 = LINE ( 'NONE', #10613, #1179 ) ;
#6554 = ORIENTED_EDGE ( 'NONE', *, *, #15595, .F. ) ;
#6555 = CARTESIAN_POINT ( 'NONE',  ( -3.000000000000000000, 3.673940397442059868E-16, 13.31572692736085095 ) ) ;
#6556 = CARTESIAN_POINT ( 'NONE',  ( 9.099998387031005720, -19.29508120620799971, 16.81964500401478091 ) ) ;
#6557 = CARTESIAN_POINT ( 'NONE',  ( 32.93470988637010066, -5.949778345213319497, -6.861505862736167138 ) ) ;
#6558 = DIRECTION ( 'NONE',  ( 0.000000000000000000, 0.000000000000000000, -1.000000000000000000 ) ) ;
#6559 =( BOUNDED_CURVE ( )  B_SPLINE_CURVE ( 2, ( #14592, #13122, #14670, #12100, #1057, #6578, #876, #14488, #10560 ),
 .UNSPECIFIED., .F., .T. ) 
 B_SPLINE_CURVE_WITH_KNOTS ( ( 3, 2, 2, 2, 3 ),
 ( 0.6346153846153846922, 0.6410256410256410797, 0.6538461538461538547, 0.6666666666666666297, 0.6730769230769231282 ),
 .UNSPECIFIED. ) 
 CURVE ( )  GEOMETRIC_REPRESENTATION_ITEM ( )  RATIONAL_B_SPLINE_CURVE ( ( 0.9330127018922192983, 0.9330127018922198534, 1.000000000000000000, 0.8660254037844387076, 1.000000000000000000, 0.8660254037844387076, 1.000000000000000000, 0.9330127018922187432, 0.9330127018922192983 ) ) 
 REPRESENTATION_ITEM ( '' )  );
#6560 = CARTESIAN_POINT ( 'NONE',  ( 26.27749392786457250, -6.324743385012029151, -8.283357778048662468 ) ) ;
#6561 = DIRECTION ( 'NONE',  ( -0.000000000000000000, -0.000000000000000000, 1.000000000000000000 ) ) ;
#6562 = CARTESIAN_POINT ( 'NONE',  ( 3.035766082959412415E-15, 4.618802153517010289, -0.5000000000000000000 ) ) ;
#6563 = FACE_OUTER_BOUND ( 'NONE', #1446, .T. ) ;
#6564 = CARTESIAN_POINT ( 'NONE',  ( 29.17398450417959310, -7.029842018119214941, -5.783357778048669573 ) ) ;
#6565 = CARTESIAN_POINT ( 'NONE',  ( 25.95846283556874212, -3.455553161483297053, -8.283357778048660691 ) ) ;
#6566 = CARTESIAN_POINT ( 'NONE',  ( 33.79776779778399032, -6.145605689821873163, 4.533357778048659803 ) ) ;
#6567 = ORIENTED_EDGE ( 'NONE', *, *, #13235, .F. ) ;
#6568 = ORIENTED_EDGE ( 'NONE', *, *, #5656, .F. ) ;
#6569 =( BOUNDED_CURVE ( )  B_SPLINE_CURVE ( 2, ( #14689, #11953, #2446, #3528, #17621, #5140, #7969, #13501, #6597 ),
 .UNSPECIFIED., .F., .T. ) 
 B_SPLINE_CURVE_WITH_KNOTS ( ( 3, 2, 2, 2, 3 ),
 ( 0.4038461538461538547, 0.4102564102564102422, 0.4230769230769230727, 0.4358974358974359031, 0.4423076923076923461 ),
 .UNSPECIFIED. ) 
 CURVE ( )  GEOMETRIC_REPRESENTATION_ITEM ( )  RATIONAL_B_SPLINE_CURVE ( ( 0.9330127018922194093, 0.9330127018922196314, 1.000000000000000000, 0.8660254037844387076, 1.000000000000000000, 0.8660254037844387076, 1.000000000000000000, 0.9330127018922190762, 0.9330127018922194093 ) ) 
 REPRESENTATION_ITEM ( '' )  );
#6570 = AXIS2_PLACEMENT_3D ( 'NONE', #14822, #3936, #9115 ) ;
#6571 = CARTESIAN_POINT ( 'NONE',  ( 28.71854711534694715, -4.576831098024959132, 7.939653947423662039 ) ) ;
#6572 = CARTESIAN_POINT ( 'NONE',  ( 1.500000000000000000, -10.39230484541326405, -3.000000000000000000 ) ) ;
#6573 = CARTESIAN_POINT ( 'NONE',  ( 17.71310509092289465, -19.55788671310905613, 15.89250038334901305 ) ) ;
#6574 = ADVANCED_FACE ( 'NONE', ( #11531 ), #13181, .F. ) ;
#6575 = ORIENTED_EDGE ( 'NONE', *, *, #6849, .T. ) ;
#6576 = CARTESIAN_POINT ( 'NONE',  ( -7.499998387031003411, -20.49508120620799900, -12.00000000000000000 ) ) ;
#6577 = CARTESIAN_POINT ( 'NONE',  ( -25.11802603177690330, -19.03270077640483038, 0.5379818257722508434 ) ) ;
#6578 = CARTESIAN_POINT ( 'NONE',  ( 28.16881664323204859, -6.096876348486420127, -8.283357778048664244 ) ) ;
#6579 = CARTESIAN_POINT ( 'NONE',  ( 29.65098506949083301, -2.583579140294649523, -4.705209693361160461 ) ) ;
#6580 = CARTESIAN_POINT ( 'NONE',  ( 30.40088504037531791, -1.856063607844930852, -6.453230759126464378 ) ) ;
#6581 = PLANE ( 'NONE',  #13316 ) ;
#6582 = CARTESIAN_POINT ( 'NONE',  ( 0.000000000000000000, 0.000000000000000000, 0.000000000000000000 ) ) ;
#6583 = CARTESIAN_POINT ( 'NONE',  ( 33.23365877489121090, -6.550928303235100891, 5.783357778048664244 ) ) ;
#6584 = ORIENTED_EDGE ( 'NONE', *, *, #7690, .F. ) ;
#6585 = CARTESIAN_POINT ( 'NONE',  ( 0.000000000000000000, 0.000000000000000000, -25.03750572909317285 ) ) ;
#6586 = CARTESIAN_POINT ( 'NONE',  ( 23.00000000000000000, -16.21813761408365195, 13.00000000000000178 ) ) ;
#6587 = CARTESIAN_POINT ( 'NONE',  ( 28.13873763417254992, -3.192873105281056390, 8.283357778048664244 ) ) ;
#6588 = ORIENTED_EDGE ( 'NONE', *, *, #9344, .F. ) ;
#6589 = VERTEX_POINT ( 'NONE', #672 ) ;
#6590 = ORIENTED_EDGE ( 'NONE', *, *, #340, .T. ) ;
#6591 = ADVANCED_FACE ( 'NONE', ( #4742 ), #14560, .F. ) ;
#6592 = CARTESIAN_POINT ( 'NONE',  ( 31.49429780130001433, -5.496349022752856861, 3.627061608673662896 ) ) ;
#6593 = DIRECTION ( 'NONE',  ( 0.9928203230275511881, 0.1196152422706614482, 0.000000000000000000 ) ) ;
#6594 = CARTESIAN_POINT ( 'NONE',  ( 29.97942892559193950, -4.424919740341219487, 7.939653947423662039 ) ) ;
#6595 = EDGE_CURVE ( 'NONE', #15658, #16993, #9799, .T. ) ;
#6596 = AXIS2_PLACEMENT_3D ( 'NONE', #11400, #14234, #9759 ) ;
#6597 = CARTESIAN_POINT ( 'NONE',  ( 30.08145424927873535, -6.930706697444451336, -5.783357778048663356 ) ) ;
#6598 = CARTESIAN_POINT ( 'NONE',  ( 26.31556265977298992, -7.384422263489805793, -5.783357778048663356 ) ) ;
#6599 = CARTESIAN_POINT ( 'NONE',  ( 30.81132015408399027, -5.578634341498224458, -3.627061608673668225 ) ) ;
#6600 = CARTESIAN_POINT ( 'NONE',  ( 30.60493568430522160, -6.867637522466304212, 6.453230759126467042 ) ) ;
#6601 = CARTESIAN_POINT ( 'NONE',  ( 33.09223089549517738, -4.049888575955752579, -8.283357778048662468 ) ) ;
#6602 = CARTESIAN_POINT ( 'NONE',  ( 31.83134908525019213, -4.201799933639492224, 3.283357778048664244 ) ) ;
#6603 = CARTESIAN_POINT ( 'NONE',  ( 20.00000000000000355, 7.999999999999996447, 6.000000000000000000 ) ) ;
#6604 = LINE ( 'NONE', #9159, #15151 ) ;
#6605 = ADVANCED_FACE ( 'NONE', ( #7473, #17100 ), #12996, .T. ) ;
#6606 = FILL_AREA_STYLE ('',( #16068 ) ) ;
#6607 = AXIS2_PLACEMENT_3D ( 'NONE', #3364, #13154, #7538 ) ;
#6608 = CARTESIAN_POINT ( 'NONE',  ( 33.58707084003705745, -6.498152266226123963, -5.783357778048669573 ) ) ;
#6609 = CARTESIAN_POINT ( 'NONE',  ( 32.91278983782564183, -5.325448745358647429, -7.939653947423662927 ) ) ;
#6610 = ORIENTED_EDGE ( 'NONE', *, *, #4385, .F. ) ;
#6611 = DIRECTION ( 'NONE',  ( 1.000000000000000000, 0.000000000000000000, 0.000000000000000000 ) ) ;
#6612 = AXIS2_PLACEMENT_3D ( 'NONE', #17481, #9099, #14897 ) ;
#6613 = DIRECTION ( 'NONE',  ( 0.000000000000000000, 0.000000000000000000, -1.000000000000000000 ) ) ;
#6614 = AXIS2_PLACEMENT_3D ( 'NONE', #2351, #13660, #9308 ) ;
#6615 = EDGE_LOOP ( 'NONE', ( #16898, #11139, #4322, #2199 ) ) ;
#6616 = CARTESIAN_POINT ( 'NONE',  ( 32.34358231980129261, -4.140085944684206432, 7.939653947423662039 ) ) ;
#6617 = CARTESIAN_POINT ( 'NONE',  ( 29.51982165028991645, -6.361204938940122844, -4.705209693361168455 ) ) ;
#6618 = EDGE_CURVE ( 'NONE', #10285, #17504, #13870, .T. ) ;
#6619 = CARTESIAN_POINT ( 'NONE',  ( 2.500000000000000000, 1.178949249685213863, -2.042000000000001148 ) ) ;
#6620 = DIRECTION ( 'NONE',  ( 0.000000000000000000, 0.000000000000000000, 1.000000000000000000 ) ) ;
#6621 = DIRECTION ( 'NONE',  ( 0.9928203230275512992, 0.1196152422706614898, -0.000000000000000000 ) ) ;
#6622 = VECTOR ( 'NONE', #17939, 1000.000000000000000 ) ;
#6623 = CYLINDRICAL_SURFACE ( 'NONE', #16867, 2.500000000000001776 ) ;
#6624 = CARTESIAN_POINT ( 'NONE',  ( 30.54048978798443059, -6.538043363838207611, -4.533357778048668685 ) ) ;
#6625 = EDGE_CURVE ( 'NONE', #6841, #14073, #15710, .T. ) ;
#6626 = ORIENTED_EDGE ( 'NONE', *, *, #13579, .T. ) ;
#6627 = FACE_OUTER_BOUND ( 'NONE', #4393, .T. ) ;
#6628 = CARTESIAN_POINT ( 'NONE',  ( 14.00000000000000178, -1.714505518806294835E-15, 8.700000000000001066 ) ) ;
#6629 = DIRECTION ( 'NONE',  ( -0.000000000000000000, -0.000000000000000000, -1.000000000000000000 ) ) ;
#6630 = CARTESIAN_POINT ( 'NONE',  ( 7.345582307948228973, 16.91090888051954977, -16.91488491921997195 ) ) ;
#6631 = VERTEX_POINT ( 'NONE', #15906 ) ;
#6632 = VECTOR ( 'NONE', #11908, 1000.000000000000000 ) ;
#6633 = CARTESIAN_POINT ( 'NONE',  ( 26.24565837299761739, -7.163851760794091916, -7.234565377303040279 ) ) ;
#6634 = CARTESIAN_POINT ( 'NONE',  ( 31.49429780130001788, -5.496349022752856861, -7.939653947423662927 ) ) ;
#6635 = VECTOR ( 'NONE', #17714, 1000.000000000000114 ) ;
#6636 = CARTESIAN_POINT ( 'NONE',  ( 32.34167700165585302, -2.686501913001913433, -8.283357778048660691 ) ) ;
#6637 = EDGE_LOOP ( 'NONE', ( #10350, #6947, #13950, #4960, #7055 ) ) ;
#6638 = CYLINDRICAL_SURFACE ( 'NONE', #19, 2.499999999999999112 ) ;
#6639 = EDGE_LOOP ( 'NONE', ( #4637, #568, #3040, #13649, #8111 ) ) ;
#6640 = CARTESIAN_POINT ( 'NONE',  ( 45.50000000000000000, -16.03270077640482683, -5.537981825772250843 ) ) ;
#6641 = CIRCLE ( 'NONE', #8685, 5.000000000000000000 ) ;
#6642 = PRODUCT_DEFINITION_SHAPE ( 'NONE', 'NONE',  #17973 ) ;
#6643 =( BOUNDED_CURVE ( )  B_SPLINE_CURVE ( 2, ( #7612, #4964, #13137, #10305, #6050, #15861, #716, #17333, #6241 ),
 .UNSPECIFIED., .F., .T. ) 
 B_SPLINE_CURVE_WITH_KNOTS ( ( 3, 2, 2, 2, 3 ),
 ( 0.8269230769230769829, 0.8333333333333333703, 0.8461538461538461453, 0.8589743589743589203, 0.8653846153846154188 ),
 .UNSPECIFIED. ) 
 CURVE ( )  GEOMETRIC_REPRESENTATION_ITEM ( )  RATIONAL_B_SPLINE_CURVE ( ( 0.9330127018922192983, 0.9330127018922198534, 1.000000000000000000, 0.8660254037844387076, 1.000000000000000000, 0.8660254037844387076, 1.000000000000000000, 0.9330127018922187432, 0.9330127018922192983 ) ) 
 REPRESENTATION_ITEM ( '' )  );
#6644 = CARTESIAN_POINT ( 'NONE',  ( 32.91278983782564183, -5.325448745358647429, -7.939653947423662927 ) ) ;
#6645 = CARTESIAN_POINT ( 'NONE',  ( -3.538288549924106796, -15.34800872113743431, -16.99955934415556769 ) ) ;
#6646 = VERTEX_POINT ( 'NONE', #3479 ) ;
#6647 = CARTESIAN_POINT ( 'NONE',  ( 33.42946061375642586, -6.517141185936593750, -5.783357778048668685 ) ) ;
#6648 = CARTESIAN_POINT ( 'NONE',  ( 26.01595305975170547, -2.384361315936983416, -5.783357778048670461 ) ) ;
#6649 = FACE_OUTER_BOUND ( 'NONE', #3453, .T. ) ;
#6650 = CARTESIAN_POINT ( 'NONE',  ( 28.08810621022444920, -4.652786776866828511, -3.627061608673664672 ) ) ;
#6651 = EDGE_CURVE ( 'NONE', #16479, #7462, #13929, .T. ) ;
#6652 = CARTESIAN_POINT ( 'NONE',  ( 32.92339180097568629, -5.524043937428110063, 8.283357778048658915 ) ) ;
#6653 = AXIS2_PLACEMENT_3D ( 'NONE', #4749, #8927, #3589 ) ;
#6654 = VECTOR ( 'NONE', #46, 1000.000000000000000 ) ;
#6655 = EDGE_CURVE ( 'NONE', #8205, #17076, #4316, .T. ) ;
#6656 = CARTESIAN_POINT ( 'NONE',  ( 29.03376756790819613, -4.538853258604016006, 3.627061608673664228 ) ) ;
#6657 = FACE_OUTER_BOUND ( 'NONE', #8161, .T. ) ;
#6658 = CARTESIAN_POINT ( 'NONE',  ( 16.75000000000000000, -16.21813761408365195, 16.03574476417184513 ) ) ;
#6659 = VERTEX_POINT ( 'NONE', #16005 ) ;
#6660 = DIRECTION ( 'NONE',  ( 0.000000000000000000, 0.000000000000000000, 1.000000000000000000 ) ) ;
#6661 = ORIENTED_EDGE ( 'NONE', *, *, #3647, .F. ) ;
#6662 = DIRECTION ( 'NONE',  ( 0.000000000000000000, 0.000000000000000000, -1.000000000000000000 ) ) ;
#6663 =( BOUNDED_CURVE ( )  B_SPLINE_CURVE ( 2, ( #11086, #5746, #16839, #4402, #10463, #687, #1964, #10194, #3401 ),
 .UNSPECIFIED., .F., .T. ) 
 B_SPLINE_CURVE_WITH_KNOTS ( ( 3, 2, 2, 2, 3 ),
 ( 0.7500000000000000000, 0.7564102564102563875, 0.7692307692307692735, 0.7820512820512820484, 0.7884615384615384359 ),
 .UNSPECIFIED. ) 
 CURVE ( )  GEOMETRIC_REPRESENTATION_ITEM ( )  RATIONAL_B_SPLINE_CURVE ( ( 0.9330127018922194093, 0.9330127018922194093, 1.000000000000000000, 0.8660254037844387076, 1.000000000000000000, 0.8660254037844387076, 1.000000000000000000, 0.9330127018922194093, 0.9330127018922194093 ) ) 
 REPRESENTATION_ITEM ( '' )  );
#6664 = VERTEX_POINT ( 'NONE', #10266 ) ;
#6665 = CARTESIAN_POINT ( 'NONE',  ( -35.62429925076629189, -17.76690233603958902, -0.5379818257722508434 ) ) ;
#6666 = CIRCLE ( 'NONE', #2354, 3.000000000000000000 ) ;
#6667 = VECTOR ( 'NONE', #15281, 1000.000000000000114 ) ;
#6668 = CARTESIAN_POINT ( 'NONE',  ( 28.91547068018125799, -2.672194098943493135, -6.861505862736158257 ) ) ;
#6669 = DIRECTION ( 'NONE',  ( 0.000000000000000000, 0.000000000000000000, -1.000000000000000000 ) ) ;
#6670 = CARTESIAN_POINT ( 'NONE',  ( 28.13873763417255347, -3.192873105281056390, -3.283357778048662023 ) ) ;
#6671 = CARTESIAN_POINT ( 'NONE',  ( 27.30005507882132676, -4.747731375419166788, 7.939653947423662039 ) ) ;
#6672 = CARTESIAN_POINT ( 'NONE',  ( 29.36638131047866196, -1.990897739957422807, 5.783357778048668685 ) ) ;
#6673 = EDGE_CURVE ( 'NONE', #7694, #5110, #9101, .T. ) ;
#6674 = CARTESIAN_POINT ( 'NONE',  ( 20.25000000000001066, -16.21813761408365195, 13.00000000000000355 ) ) ;
#6675 = CARTESIAN_POINT ( 'NONE',  ( 32.24155699611449677, -1.634298987580965923, 5.783357778048662468 ) ) ;
#6676 = CARTESIAN_POINT ( 'NONE',  ( 32.18597209352066812, -4.159074864394664672, 3.627061608673664228 ) ) ;
#6677 = VERTEX_POINT ( 'NONE', #7739 ) ;
#6678 = CARTESIAN_POINT ( 'NONE',  ( 28.55903157092087952, -3.142235986053133256, 3.283357778048666464 ) ) ;
#6679 = ORIENTED_EDGE ( 'NONE', *, *, #7482, .T. ) ;
#6680 = ORIENTED_EDGE ( 'NONE', *, *, #10725, .F. ) ;
#6681 = CARTESIAN_POINT ( 'NONE',  ( 33.30246708102489350, -5.905470865888903020, 6.861505862736158257 ) ) ;
#6682 = CARTESIAN_POINT ( 'NONE',  ( 28.82057243903374655, -7.082618055128190093, -5.783357778048668685 ) ) ;
#6683 = CARTESIAN_POINT ( 'NONE',  ( 29.55043834383900148, -5.730545699181964991, 7.939653947423658487 ) ) ;
#6684 = ORIENTED_EDGE ( 'NONE', *, *, #7138, .F. ) ;
#6685 = CARTESIAN_POINT ( 'NONE',  ( 30.25524682244395436, -4.391689130744175884, 8.283357778048662468 ) ) ;
#6686 = VECTOR ( 'NONE', #14611, 1000.000000000000000 ) ;
#6687 = CARTESIAN_POINT ( 'NONE',  ( -2.016448651773435938E-27, -20.49999999999999645, 12.00000000000000000 ) ) ;
#6688 = CARTESIAN_POINT ( 'NONE',  ( 27.58784498402260610, -7.231137369010889770, -6.453230759126474148 ) ) ;
#6689 = FACE_OUTER_BOUND ( 'NONE', #10611, .T. ) ;
#6690 = CARTESIAN_POINT ( 'NONE',  ( 26.21851383115118495, -6.578905779530963116, -7.633279253667162756 ) ) ;
#6691 = LINE ( 'NONE', #3976, #9639 ) ;
#6692 = DIRECTION ( 'NONE',  ( -0.1196152422706610735, 0.9928203230275511881, 0.000000000000000000 ) ) ;
#6693 = CARTESIAN_POINT ( 'NONE',  ( -5.816800114226745675E-16, -4.862606272033100474, -3.445885042887441241 ) ) ;
#6694 = CARTESIAN_POINT ( 'NONE',  ( 28.68570264635560463, -13.61469575198669624, 13.53129406029897730 ) ) ;
#6695 = AXIS2_PLACEMENT_3D ( 'NONE', #15042, #6701, #16498 ) ;
#6696 = EDGE_CURVE ( 'NONE', #4963, #16104, #4614, .T. ) ;
#6697 = CARTESIAN_POINT ( 'NONE',  ( 32.29974222271236073, -2.891426744974864071, -3.627061608673662008 ) ) ;
#6698 = CARTESIAN_POINT ( 'NONE',  ( 29.55043834383900148, -5.730545699181964991, -3.627061608673668225 ) ) ;
#6699 = CARTESIAN_POINT ( 'NONE',  ( 31.15208055228630357, -2.102918000029084578, 7.033357778048666020 ) ) ;
#6700 = AXIS2_PLACEMENT_3D ( 'NONE', #2045, #7571, #2878 ) ;
#6701 = DIRECTION ( 'NONE',  ( -0.000000000000000000, -0.000000000000000000, -1.000000000000000000 ) ) ;
#6702 = ORIENTED_EDGE ( 'NONE', *, *, #419, .F. ) ;
#6703 = ORIENTED_EDGE ( 'NONE', *, *, #7938, .T. ) ;
#6704 = CARTESIAN_POINT ( 'NONE',  ( 30.45225960443380231, -4.367952981209816343, 7.939653947423662039 ) ) ;
#6705 = CONICAL_SURFACE ( 'NONE', #1219, 2.055000000000000160, 0.7853981633974794763 ) ;
#6706 = CARTESIAN_POINT ( 'NONE',  ( 27.09860475545177039, -3.518061095420291995, -3.627061608673662896 ) ) ;
#6707 = CARTESIAN_POINT ( 'NONE',  ( 32.55256711014040150, -6.632986398338614364, -6.453230759126470595 ) ) ;
#6708 = DIRECTION ( 'NONE',  ( -0.05980762113533041185, 0.4964101615137757606, -0.8660254037844384856 ) ) ;
#6709 = DIRECTION ( 'NONE',  ( -1.000000000000000000, 0.000000000000000000, 0.000000000000000000 ) ) ;
#6710 = DIRECTION ( 'NONE',  ( 0.9928203230275510771, 0.1196152422706614621, -0.000000000000000000 ) ) ;
#6711 = VECTOR ( 'NONE', #832, 1000.000000000000000 ) ;
#6712 = CARTESIAN_POINT ( 'NONE',  ( 1.746467850512308208E-21, -1.591841644184202181E-21, -6.005572809000082835 ) ) ;
#6713 = CARTESIAN_POINT ( 'NONE',  ( 27.24942365487322959, -6.207645047004941574, -3.283357778048667797 ) ) ;
#6714 = ORIENTED_EDGE ( 'NONE', *, *, #12545, .T. ) ;
#6715 = CARTESIAN_POINT ( 'NONE',  ( 0.2500000000000002220, 0.000000000000000000, 0.000000000000000000 ) ) ;
#6716 = AXIS2_PLACEMENT_3D ( 'NONE', #11636, #10356, #676 ) ;
#6717 = CARTESIAN_POINT ( 'NONE',  ( 33.95908713831674675, -3.945449517755637903, 5.783357778048663356 ) ) ;
#6718 = CARTESIAN_POINT ( 'NONE',  ( 30.58169613980036772, -2.898544849976259385, 8.283357778048666020 ) ) ;
#6719 = CARTESIAN_POINT ( 'NONE',  ( 10.50000000000000000, 1.285879139104720831E-15, -7.794427190999915211 ) ) ;
#6720 = EDGE_CURVE ( 'NONE', #11483, #13130, #17211, .T. ) ;
#6721 = CARTESIAN_POINT ( 'NONE',  ( 28.35948656569676629, -3.366149737736551906, -3.627061608673662896 ) ) ;
#6722 = CIRCLE ( 'NONE', #12243, 0.9000000000000003553 ) ;
#6723 = VECTOR ( 'NONE', #1327, 1000.000000000000227 ) ;
#6724 = VECTOR ( 'NONE', #8888, 1000.000000000000000 ) ;
#6725 = EDGE_CURVE ( 'NONE', #15379, #13857, #3909, .T. ) ;
#6726 = DIRECTION ( 'NONE',  ( 1.000000000000000000, 0.000000000000000000, 0.000000000000000000 ) ) ;
#6727 = CARTESIAN_POINT ( 'NONE',  ( -26.11885528537984413, -10.78654967147420329, -14.20677827292374040 ) ) ;
#6728 = ORIENTED_EDGE ( 'NONE', *, *, #8192, .F. ) ;
#6729 = CARTESIAN_POINT ( 'NONE',  ( 25.80383423833348999, -3.137017275366889457, 4.425119566059311893 ) ) ;
#6730 = VERTEX_POINT ( 'NONE', #17815 ) ;
#6731 = CIRCLE ( 'NONE', #14277, 0.9000000000000003553 ) ;
#6732 = CARTESIAN_POINT ( 'NONE',  ( 31.03886041246737548, -3.043338102658604161, -3.627061608673662008 ) ) ;
#6733 = FACE_OUTER_BOUND ( 'NONE', #14725, .T. ) ;
#6734 = AXIS2_PLACEMENT_3D ( 'NONE', #5293, #12460, #15269 ) ;
#6735 = VERTEX_POINT ( 'NONE', #8165 ) ;
#6736 = CIRCLE ( 'NONE', #1209, 10.50000000000000000 ) ;
#6737 = EDGE_LOOP ( 'NONE', ( #5805, #12459 ) ) ;
#6738 = CARTESIAN_POINT ( 'NONE',  ( 26.03726795043090547, -3.446058701420613879, -8.283357778048658915 ) ) ;
#6739 = CARTESIAN_POINT ( 'NONE',  ( 31.59864285835955400, -2.049116061056871274, 4.533357778048667797 ) ) ;
#6740 = CARTESIAN_POINT ( 'NONE',  ( 0.000000000000000000, 0.000000000000000000, -25.03750572909317285 ) ) ;
#6741 = CARTESIAN_POINT ( 'NONE',  ( 33.79776779778399032, -6.145605689821873163, -7.033357778048666908 ) ) ;
#6742 = EDGE_CURVE ( 'NONE', #17907, #2702, #4077, .T. ) ;
#6743 = ORIENTED_EDGE ( 'NONE', *, *, #4901, .T. ) ;
#6744 = CARTESIAN_POINT ( 'NONE',  ( 30.07408527595748282, -27.82894256842317660, 13.18310524188698452 ) ) ;
#6745 = CIRCLE ( 'NONE', #13428, 10.50000000000000000 ) ;
#6746 = ORIENTED_EDGE ( 'NONE', *, *, #11581, .T. ) ;
#6747 = AXIS2_PLACEMENT_3D ( 'NONE', #6379, #13457, #10537 ) ;
#6748 = VECTOR ( 'NONE', #5709, 1000.000000000000114 ) ;
#6749 = EDGE_CURVE ( 'NONE', #3447, #16316, #6129, .T. ) ;
#6750 =( BOUNDED_CURVE ( )  B_SPLINE_CURVE ( 2, ( #6938, #8570, #13919, #11364, #15468, #1328, #4143, #6852, #2778 ),
 .UNSPECIFIED., .F., .T. ) 
 B_SPLINE_CURVE_WITH_KNOTS ( ( 3, 2, 2, 2, 3 ),
 ( 0.8269230769230769829, 0.8333333333333333703, 0.8461538461538461453, 0.8589743589743589203, 0.8653846153846154188 ),
 .UNSPECIFIED. ) 
 CURVE ( )  GEOMETRIC_REPRESENTATION_ITEM ( )  RATIONAL_B_SPLINE_CURVE ( ( 0.9330127018922192983, 0.9330127018922198534, 1.000000000000000000, 0.8660254037844387076, 1.000000000000000000, 0.8660254037844387076, 1.000000000000000000, 0.9330127018922187432, 0.9330127018922192983 ) ) 
 REPRESENTATION_ITEM ( '' )  );
#6751 = CARTESIAN_POINT ( 'NONE',  ( 29.76058531221316628, -5.705227139567997874, 3.627061608673662896 ) ) ;
#6752 = DIRECTION ( 'NONE',  ( -0.5999999999999999778, -0.7999999999999999334, -0.000000000000000000 ) ) ;
#6753 = CARTESIAN_POINT ( 'NONE',  ( 25.01460733971720529, -22.13799366862516038, 14.47321228143779415 ) ) ;
#6754 = ORIENTED_EDGE ( 'NONE', *, *, #16115, .T. ) ;
#6755 = DIRECTION ( 'NONE',  ( -1.000000000000000000, 0.000000000000000000, 0.000000000000000000 ) ) ;
#6756 = ORIENTED_EDGE ( 'NONE', *, *, #14708, .F. ) ;
#6757 = FACE_OUTER_BOUND ( 'NONE', #5954, .T. ) ;
#6758 = EDGE_CURVE ( 'NONE', #1259, #13758, #12508, .T. ) ;
#6759 = ORIENTED_EDGE ( 'NONE', *, *, #10386, .T. ) ;
#6760 = DIRECTION ( 'NONE',  ( -1.000000000000000000, 0.000000000000000000, 0.000000000000000000 ) ) ;
#6761 = CARTESIAN_POINT ( 'NONE',  ( 28.89355063163679915, -2.047864499088824175, -5.783357778048658027 ) ) ;
#6762 = AXIS2_PLACEMENT_3D ( 'NONE', #601, #17911, #3600 ) ;
#6763 = CARTESIAN_POINT ( 'NONE',  ( 26.56758885001203652, -2.317900097157796324, 5.783357778048657138 ) ) ;
#6764 = DIRECTION ( 'NONE',  ( 1.000000000000000000, 0.000000000000000000, 0.000000000000000000 ) ) ;
#6765 = CARTESIAN_POINT ( 'NONE',  ( 32.41296236253129592, -1.951006642345344044, 7.033357778048666020 ) ) ;
#6766 = CARTESIAN_POINT ( 'NONE',  ( 30.15026255541241440, -6.285249260098253465, 6.861505862736158257 ) ) ;
#6767 = EDGE_CURVE ( 'NONE', #8284, #15182, #17092, .T. ) ;
#6768 = CARTESIAN_POINT ( 'NONE',  ( 25.89690931182567724, -3.909551132893385184, -5.783357778048664244 ) ) ;
#6769 = CARTESIAN_POINT ( 'NONE',  ( 27.27683486999669427, -2.232449958253242883, -5.783357778048658027 ) ) ;
#6770 = DIRECTION ( 'NONE',  ( -0.000000000000000000, -1.000000000000000000, 3.469446951953614189E-16 ) ) ;
#6771 = ORIENTED_EDGE ( 'NONE', *, *, #9109, .T. ) ;
#6772 = ORIENTED_EDGE ( 'NONE', *, *, #3245, .F. ) ;
#6773 = CARTESIAN_POINT ( 'NONE',  ( 31.93198502805756789, -2.935734224299280548, 3.627061608673666893 ) ) ;
#6774 = FACE_OUTER_BOUND ( 'NONE', #13628, .T. ) ;
#6775 = ORIENTED_EDGE ( 'NONE', *, *, #16237, .T. ) ;
#6776 = CARTESIAN_POINT ( 'NONE',  ( 28.91999743871649997, -5.806501378023834370, 7.939653947423658487 ) ) ;
#6777 = ORIENTED_EDGE ( 'NONE', *, *, #4107, .F. ) ;
#6778 = FACE_BOUND ( 'NONE', #3110, .T. ) ;
#6779 = FACE_OUTER_BOUND ( 'NONE', #4172, .T. ) ;
#6780 = ADVANCED_FACE ( 'NONE', ( #9506 ), #4261, .T. ) ;
#6781 = ORIENTED_EDGE ( 'NONE', *, *, #2157, .F. ) ;
#6782 = CARTESIAN_POINT ( 'NONE',  ( 29.98885399772409954, -6.604504582617394703, -4.533357778048668685 ) ) ;
#6783 = CARTESIAN_POINT ( 'NONE',  ( 26.01595305975170547, -2.384361315936983416, -5.783357778048670461 ) ) ;
#6784 = DIRECTION ( 'NONE',  ( 0.9928203230275511881, 0.1196152422706614482, 0.000000000000000000 ) ) ;
#6785 = CARTESIAN_POINT ( 'NONE',  ( 31.32102116884452414, -5.717097954277069682, -8.283357778048662468 ) ) ;
#6786 = DIRECTION ( 'NONE',  ( -0.1196152422706610735, 0.9928203230275511881, 0.000000000000000000 ) ) ;
#6787 = CARTESIAN_POINT ( 'NONE',  ( 28.92482766011098150, -14.18604173879621477, -13.46461621778217577 ) ) ;
#6788 = FACE_OUTER_BOUND ( 'NONE', #11326, .T. ) ;
#6789 = VERTEX_POINT ( 'NONE', #12599 ) ;
#6790 = EDGE_LOOP ( 'NONE', ( #1976, #15935, #560, #14603 ) ) ;
#6791 = EDGE_CURVE ( 'NONE', #11389, #2070, #16686, .T. ) ;
#6792 = CARTESIAN_POINT ( 'NONE',  ( 32.50119254608192421, -4.121097024973739309, -3.627061608673664672 ) ) ;
#6793 = CARTESIAN_POINT ( 'NONE',  ( 27.25621498173240198, -3.499072175709823984, -3.627061608673662008 ) ) ;
#6794 = VERTEX_POINT ( 'NONE', #8518 ) ;
#6795 = LINE ( 'NONE', #17888, #9767 ) ;
#6796 = CARTESIAN_POINT ( 'NONE',  ( 0.000000000000000000, 0.000000000000000000, -4.699999999999999289 ) ) ;
#6797 = PRODUCT_DEFINITION_SHAPE ( 'NONE', 'NONE',  #17977 ) ;
#6798 = VERTEX_POINT ( 'NONE', #12247 ) ;
#6799 = CARTESIAN_POINT ( 'NONE',  ( 33.38562051666750818, -5.268481986227246949, 3.627061608673662896 ) ) ;
#6800 = CARTESIAN_POINT ( 'NONE',  ( 27.08121146544255353, -6.028038774645947839, -7.939653947423662927 ) ) ;
#6801 = DIRECTION ( 'NONE',  ( 0.000000000000000000, 0.000000000000000000, 1.000000000000000000 ) ) ;
#6802 = EDGE_CURVE ( 'NONE', #1572, #729, #4335, .T. ) ;
#6803 = CARTESIAN_POINT ( 'NONE',  ( 27.87912141988533676, -2.159886323212414361, 5.113484796970856117 ) ) ;
#6804 = CARTESIAN_POINT ( 'NONE',  ( 30.88577694472199298, -6.196634301449400084, -6.861505862736166250 ) ) ;
#6805 = DIRECTION ( 'NONE',  ( -0.000000000000000000, -0.000000000000000000, 1.000000000000000000 ) ) ;
#6806 = EDGE_CURVE ( 'NONE', #15344, #10032, #9856, .T. ) ;
#6807 = CARTESIAN_POINT ( 'NONE',  ( 28.79241808379989465, -7.086010098929231837, -5.113484796970862334 ) ) ;
#6808 = CARTESIAN_POINT ( 'NONE',  ( 32.60321786976872005, -6.626883982076972046, -5.783357778048663356 ) ) ;
#6809 = UNCERTAINTY_MEASURE_WITH_UNIT (LENGTH_MEASURE( 1.000000000000000082E-05 ), #9663, 'distance_accuracy_value', 'NONE');
#6810 = CARTESIAN_POINT ( 'NONE',  ( 28.72045243349238675, -6.030415129707233035, -8.283357778048662468 ) ) ;
#6811 = VERTEX_POINT ( 'NONE', #5601 ) ;
#6812 = CONTEXT_DEPENDENT_SHAPE_REPRESENTATION ( #2300, #4893 ) ;
#6813 = CARTESIAN_POINT ( 'NONE',  ( 31.93198502805756789, -2.935734224299280548, -7.939653947423660263 ) ) ;
#6814 = LINE ( 'NONE', #2815, #16843 ) ;
#6815 = CARTESIAN_POINT ( 'NONE',  ( 26.70901672940806648, -4.818939824437135755, -8.283357778048662468 ) ) ;
#6816 = DIRECTION ( 'NONE',  ( -0.1196152422706611984, 0.9928203230275510771, 0.000000000000000000 ) ) ;
#6817 = LINE ( 'NONE', #12342, #3426 ) ;
#6818 = CARTESIAN_POINT ( 'NONE',  ( 29.51982165028991645, -6.361204938940122844, -4.705209693361168455 ) ) ;
#6819 = ORIENTED_EDGE ( 'NONE', *, *, #8675, .T. ) ;
#6820 = CARTESIAN_POINT ( 'NONE',  ( 32.46178999037268653, -4.125844254797621957, -8.283357778048662468 ) ) ;
#6821 = CARTESIAN_POINT ( 'NONE',  ( -29.20850947011023280, -15.38975055298431549, -13.38439523458337099 ) ) ;
#6822 = ORIENTED_EDGE ( 'NONE', *, *, #15074, .T. ) ;
#6823 = EDGE_CURVE ( 'NONE', #4105, #6239, #12130, .T. ) ;
#6824 = CARTESIAN_POINT ( 'NONE',  ( 29.66420847303068697, -4.462897579762144851, -7.939653947423662039 ) ) ;
#6825 = CARTESIAN_POINT ( 'NONE',  ( 20.00000000000000355, 7.999999999999996447, 6.000000000000000000 ) ) ;
#6826 = ORIENTED_EDGE ( 'NONE', *, *, #608, .F. ) ;
#6827 = CARTESIAN_POINT ( 'NONE',  ( 27.60595198473284384, -7.618504009027492252, -5.783357778048669573 ) ) ;
#6828 = EDGE_CURVE ( 'NONE', #5257, #9208, #11742, .T. ) ;
#6829 = CARTESIAN_POINT ( 'NONE',  ( 31.90644508241650357, -6.373472726347483963, 4.533357778048659803 ) ) ;
#6830 = CARTESIAN_POINT ( 'NONE',  ( 4.000000000000000000, -2.471526491860382091, -3.386887032901836125 ) ) ;
#6831 = CARTESIAN_POINT ( 'NONE',  ( 27.88665588685489993, -3.423116496867954162, -3.627061608673662008 ) ) ;
#6832 = CARTESIAN_POINT ( 'NONE',  ( 24.62797819841904001, -22.25577170577939157, -14.56336204217505426 ) ) ;
#6833 = CARTESIAN_POINT ( 'NONE',  ( 26.63030083514515312, -6.709335133632020387, 4.705209693361159573 ) ) ;
#6834 = CARTESIAN_POINT ( 'NONE',  ( -45.00000000000000711, -19.03270077640483038, -0.5379818257722508434 ) ) ;
#6835 = CARTESIAN_POINT ( 'NONE',  ( -4.211140560182196957, 2.431303136016540911, -3.445885042887435468 ) ) ;
#6836 = ORIENTED_EDGE ( 'NONE', *, *, #16676, .T. ) ;
#6837 = CARTESIAN_POINT ( 'NONE',  ( 28.52524344760924180, -2.419399995203538101, 4.533357778048667797 ) ) ;
#6838 = VERTEX_POINT ( 'NONE', #8703 ) ;
#6839 = CARTESIAN_POINT ( 'NONE',  ( 1.500000000000000666, 5.809475019311125976, -2.000000000000000000 ) ) ;
#6840 = EDGE_CURVE ( 'NONE', #6841, #9483, #3262, .T. ) ;
#6841 = VERTEX_POINT ( 'NONE', #12955 ) ;
#6842 = DIRECTION ( 'NONE',  ( 0.8660254037844329345, -0.5000000000000099920, 0.000000000000000000 ) ) ;
#6843 = CARTESIAN_POINT ( 'NONE',  ( 28.93739072872572393, -3.296523698798161650, -7.939653947423660263 ) ) ;
#6844 = PRODUCT_DEFINITION_CONTEXT ( 'detailed design', #15714, 'design' ) ;
#6845 = CARTESIAN_POINT ( 'NONE',  ( -25.11802603177690330, -19.03270077640483038, 0.5379818257722508434 ) ) ;
#6846 = DIRECTION ( 'NONE',  ( 1.000000000000000000, 0.000000000000000000, 0.000000000000000000 ) ) ;
#6847 = DIRECTION ( 'NONE',  ( 0.000000000000000000, 0.000000000000000000, 1.000000000000000000 ) ) ;
#6848 = CARTESIAN_POINT ( 'NONE',  ( 26.36761712467744090, -6.740983333149474177, 6.861505862736158257 ) ) ;
#6849 = EDGE_CURVE ( 'NONE', #14109, #6677, #13309, .T. ) ;
#6850 = CARTESIAN_POINT ( 'NONE',  ( 30.86385689617752348, -5.572304701594726239, 3.627061608673662896 ) ) ;
#6851 = FACE_OUTER_BOUND ( 'NONE', #10203, .T. ) ;
#6852 = CARTESIAN_POINT ( 'NONE',  ( 26.04410741498555382, -2.380969272135942560, -5.113484796970857893 ) ) ;
#6853 = DIRECTION ( 'NONE',  ( -1.000000000000000000, 0.000000000000000000, 0.000000000000000000 ) ) ;
#6854 = VERTEX_POINT ( 'NONE', #13045 ) ;
#6855 = ORIENTED_EDGE ( 'NONE', *, *, #2531, .F. ) ;
#6856 = ORIENTED_EDGE ( 'NONE', *, *, #4191, .F. ) ;
#6857 = B_SPLINE_CURVE_WITH_KNOTS ( 'NONE', 3,
 ( #6106, #9106, #9014, #10270 ),
 .UNSPECIFIED., .F., .F.,
 ( 4, 4 ),
 ( 2.843119637709864978E-07, 0.001422633878257846410 ),
 .UNSPECIFIED. ) ;
#6858 = CARTESIAN_POINT ( 'NONE',  ( 30.76748005699505129, -4.329975141788874993, 3.627061608673664228 ) ) ;
#6859 = LINE ( 'NONE', #12385, #14843 ) ;
#6860 = ORIENTED_EDGE ( 'NONE', *, *, #3449, .T. ) ;
#6861 = CARTESIAN_POINT ( 'NONE',  ( 29.02054416436834217, -2.659534819136519790, 6.861505862736166250 ) ) ;
#6862 = CARTESIAN_POINT ( 'NONE',  ( 26.27749392786456895, -6.324743385012030927, -8.283357778048664244 ) ) ;
#6863 = DIRECTION ( 'NONE',  ( 0.000000000000000000, 0.000000000000000000, 1.000000000000000000 ) ) ;
#6864 = EDGE_LOOP ( 'NONE', ( #5375, #1214, #10764 ) ) ;
#6865 = CARTESIAN_POINT ( 'NONE',  ( 30.61929490284659394, -6.528548903775525325, -4.533357778048668685 ) ) ;
#6866 = LINE ( 'NONE', #11019, #12810 ) ;
#6867 = CIRCLE ( 'NONE', #12066, 2.499999999999999556 ) ;
#6868 = CARTESIAN_POINT ( 'NONE',  ( 0.3461262719736145632, -4.658553426539295828, -3.371615880910378671 ) ) ;
#6869 = CARTESIAN_POINT ( 'NONE',  ( 29.20802265909081896, -15.38590642643731066, 13.38453386482100171 ) ) ;
#6870 = SHAPE_REPRESENTATION_RELATIONSHIP ( 'NONE' , 'NONE' ,  #2651, #7664 ) ;
#6871 = CARTESIAN_POINT ( 'NONE',  ( 29.66420847303068697, -4.462897579762144851, -7.939653947423662039 ) ) ;
#6872 = CARTESIAN_POINT ( 'NONE',  ( 27.45766530510195835, -4.728742455708699666, -3.627061608673664672 ) ) ;
#6873 = ORIENTED_EDGE ( 'NONE', *, *, #1767, .T. ) ;
#6874 = CARTESIAN_POINT ( 'NONE',  ( -5.500000000000000000, -20.49999999999999645, 6.000000000000000000 ) ) ;
#6875 = ADVANCED_FACE ( 'NONE', ( #4787 ), #11401, .F. ) ;
#6876 = DIRECTION ( 'NONE',  ( 1.000000000000000000, -1.734723475976805517E-15, 0.000000000000000000 ) ) ;
#6877 = VERTEX_POINT ( 'NONE', #3349 ) ;
#6878 = AXIS2_PLACEMENT_3D ( 'NONE', #5820, #15534, #5550 ) ;
#6879 = ORIENTED_EDGE ( 'NONE', *, *, #15699, .F. ) ;
#6880 = CARTESIAN_POINT ( 'NONE',  ( 31.28415083292585663, -5.521667582366822202, 7.939653947423658487 ) ) ;
#6881 = CARTESIAN_POINT ( 'NONE',  ( 28.38593337277646711, -7.124786616671554107, -5.783357778048668685 ) ) ;
#6882 = CARTESIAN_POINT ( 'NONE',  ( 32.96626681528915981, -4.065064760026301016, 5.783357778048663356 ) ) ;
#6883 = CARTESIAN_POINT ( 'NONE',  ( -20.25000000000000711, -16.21813761408365195, 13.00000000000000178 ) ) ;
#6884 = EDGE_CURVE ( 'NONE', #9143, #2135, #13607, .T. ) ;
#6885 = VERTEX_POINT ( 'NONE', #14330 ) ;
#6886 = CARTESIAN_POINT ( 'NONE',  ( -20.00000000000000355, 7.999999999999996447, 0.000000000000000000 ) ) ;
#6887 = CARTESIAN_POINT ( 'NONE',  ( 28.23249303296521617, -2.754479417688857179, -4.705209693361161349 ) ) ;
#6888 = CARTESIAN_POINT ( 'NONE',  ( 32.46178999037268653, -4.125844254797621957, 3.283357778048664244 ) ) ;
#6889 = DIRECTION ( 'NONE',  ( 0.9928203230275510771, 0.1196152422706609902, 4.006172263299092517E-17 ) ) ;
#6890 = DIRECTION ( 'NONE',  ( 0.000000000000000000, 0.000000000000000000, 1.000000000000000000 ) ) ;
#6891 = CARTESIAN_POINT ( 'NONE',  ( 29.11066736118121057, -3.075774767273946608, -8.283357778048658915 ) ) ;
#6892 = AXIS2_PLACEMENT_3D ( 'NONE', #16095, #13780, #7737 ) ;
#6893 = EDGE_LOOP ( 'NONE', ( #6079, #8981, #18, #4844 ) ) ;
#6894 = CARTESIAN_POINT ( 'NONE',  ( 29.41022140756759029, -3.239556939666760726, -7.939653947423660263 ) ) ;
#6895 = CIRCLE ( 'NONE', #17053, 2.749999999999988454 ) ;
#6896 = FILL_AREA_STYLE ('',( #13791 ) ) ;
#6897 = CARTESIAN_POINT ( 'NONE',  ( 33.66004903264009585, -1.463398710186758267, -5.783357778048663356 ) ) ;
#6898 = DIRECTION ( 'NONE',  ( 0.000000000000000000, 0.000000000000000000, 1.000000000000000000 ) ) ;
#6899 = FACE_OUTER_BOUND ( 'NONE', #6204, .T. ) ;
#6900 = EDGE_CURVE ( 'NONE', #4898, #16224, #4522, .T. ) ;
#6901 = CARTESIAN_POINT ( 'NONE',  ( 27.61527553138257574, -4.709753535998224550, -7.939653947423662039 ) ) ;
#6902 = VECTOR ( 'NONE', #107, 1000.000000000000000 ) ;
#6903 = VERTEX_POINT ( 'NONE', #8881 ) ;
#6904 = CARTESIAN_POINT ( 'NONE',  ( 4.000000000000000000, 2.309401076758510918, -0.5000000000000000000 ) ) ;
#6905 = CARTESIAN_POINT ( 'NONE',  ( 5.781152949374518180, -1.605699403978931405, -2.000000000000000000 ) ) ;
#6906 = AXIS2_PLACEMENT_3D ( 'NONE', #8581, #247, #6951 ) ;
#6907 = ORIENTED_EDGE ( 'NONE', *, *, #1216, .T. ) ;
#6908 = DIRECTION ( 'NONE',  ( 0.9928203230275512992, 0.1196152422706614898, -0.000000000000000000 ) ) ;
#6909 = ORIENTED_EDGE ( 'NONE', *, *, #6651, .T. ) ;
#6910 = CARTESIAN_POINT ( 'NONE',  ( 30.78487334700428235, -1.819997462563214263, -5.783357778048658915 ) ) ;
#6911 = CARTESIAN_POINT ( 'NONE',  ( 4.024499207728657879, 2.323545700935572000, -3.272172305156507921 ) ) ;
#6912 = CARTESIAN_POINT ( 'NONE',  ( 25.52694003402523748, -4.961356722058193114, -8.283357778048662468 ) ) ;
#6913 = CARTESIAN_POINT ( 'NONE',  ( -20.25000000000000355, -16.21813761408365195, 0.000000000000000000 ) ) ;
#6914 = CARTESIAN_POINT ( 'NONE',  ( 32.51061761821408425, -6.300681867249914525, 7.033357778048657138 ) ) ;
#6915 = CARTESIAN_POINT ( 'NONE',  ( 27.23882169172318513, -6.009049854935478052, -7.939653947423664704 ) ) ;
#6916 = VECTOR ( 'NONE', #13904, 1000.000000000000000 ) ;
#6917 = EDGE_CURVE ( 'NONE', #17090, #6049, #14416, .T. ) ;
#6918 = CARTESIAN_POINT ( 'NONE',  ( 21.03881409870396624, -22.15596512169676302, -15.31966522629967464 ) ) ;
#6919 = EDGE_LOOP ( 'NONE', ( #11825, #17770, #643, #16034, #16052, #6771, #15361, #15224, #9583, #89, #10076 ) ) ;
#6920 = CARTESIAN_POINT ( 'NONE',  ( 27.26074174026764751, -6.633379454790151009, 4.705209693361159573 ) ) ;
#6921 = CARTESIAN_POINT ( 'NONE',  ( 17.31832318566733164, -18.83027996791590652, 15.95242868103980172 ) ) ;
#6922 = ADVANCED_FACE ( 'NONE', ( #1998 ), #11298, .T. ) ;
#6923 = ORIENTED_EDGE ( 'NONE', *, *, #17453, .F. ) ;
#6924 = CARTESIAN_POINT ( 'NONE',  ( 30.98067518586950442, -1.786210345264705790, 5.783357778048667797 ) ) ;
#6925 = ORIENTED_EDGE ( 'NONE', *, *, #15574, .T. ) ;
#6926 = CIRCLE ( 'NONE', #5465, 2.749999999999988454 ) ;
#6927 = DIRECTION ( 'NONE',  ( 1.000000000000000000, 3.552713678800500929E-15, 0.000000000000000000 ) ) ;
#6928 = VERTEX_POINT ( 'NONE', #3164 ) ;
#6929 = FACE_OUTER_BOUND ( 'NONE', #7004, .T. ) ;
#6930 = CARTESIAN_POINT ( 'NONE',  ( 31.06530721954707985, -6.801974981593605030, -5.783357778048669573 ) ) ;
#6931 = CARTESIAN_POINT ( 'NONE',  ( 46.86575133767495061, -2.390451368237048069, -5.783357778048661579 ) ) ;
#6932 = DIRECTION ( 'NONE',  ( -1.000000000000000000, 0.000000000000000000, 0.000000000000000000 ) ) ;
#6933 = CARTESIAN_POINT ( 'NONE',  ( 0.000000000000000000, 0.000000000000000000, 9.600000000000001421 ) ) ;
#6934 = CARTESIAN_POINT ( 'NONE',  ( 33.79776779778399032, -6.145605689821873163, 4.533357778048659803 ) ) ;
#6935 = AXIS2_PLACEMENT_3D ( 'NONE', #1410, #5564, #6846 ) ;
#6936 = CARTESIAN_POINT ( 'NONE',  ( 28.24571643650507369, -4.633797857156355171, 3.627061608673664228 ) ) ;
#6937 = CARTESIAN_POINT ( 'NONE',  ( 19.43845002722867221, 2.988003976273734263, 0.000000000000000000 ) ) ;
#6938 = CARTESIAN_POINT ( 'NONE',  ( 26.92924972366625980, -7.310485091653801781, -5.783357778048657138 ) ) ;
#6939 = CARTESIAN_POINT ( 'NONE',  ( 32.17274868998081416, -2.279756424927169345, 6.861505862736166250 ) ) ;
#6940 = AXIS2_PLACEMENT_3D ( 'NONE', #4416, #9837, #6033 ) ;
#6941 = ADVANCED_FACE ( 'NONE', ( #458, #630 ), #8967, .T. ) ;
#6942 = VERTEX_POINT ( 'NONE', #14235 ) ;
#6943 = ORIENTED_EDGE ( 'NONE', *, *, #14606, .T. ) ;
#6944 = CARTESIAN_POINT ( 'NONE',  ( 28.97253418081003673, -5.800171738120336151, 3.627061608673662896 ) ) ;
#6945 = DIRECTION ( 'NONE',  ( -0.000000000000000000, -0.000000000000000000, -1.000000000000000000 ) ) ;
#6946 = ADVANCED_FACE ( 'NONE', ( #7172, #10133 ), #271, .F. ) ;
#6947 = ORIENTED_EDGE ( 'NONE', *, *, #2917, .F. ) ;
#6948 = CARTESIAN_POINT ( 'NONE',  ( 27.28266178881210280, -7.257709054644825741, 5.783357778048657138 ) ) ;
#6949 = ADVANCED_FACE ( 'NONE', ( #5783 ), #17056, .F. ) ;
#6950 = EDGE_LOOP ( 'NONE', ( #4645, #16916, #17348, #673 ) ) ;
#6951 = DIRECTION ( 'NONE',  ( 0.1196152422706608098, -0.9928203230275511881, 0.000000000000000000 ) ) ;
#6952 = FACE_OUTER_BOUND ( 'NONE', #7166, .T. ) ;
#6953 = CARTESIAN_POINT ( 'NONE',  ( 26.01652455409633902, -4.902371455920928156, -5.783357778048663356 ) ) ;
#6954 = CARTESIAN_POINT ( 'NONE',  ( 27.12922144900085186, -2.887401855662130146, -4.705209693361160461 ) ) ;
#6955 = CARTESIAN_POINT ( 'NONE',  ( 26.02974819644417792, -2.720057890826728109, -4.533357778048659803 ) ) ;
#6956 = VECTOR ( 'NONE', #8820, 1000.000000000000000 ) ;
#6957 = CARTESIAN_POINT ( 'NONE',  ( 31.08079519141086777, -2.838413270685653078, -8.283357778048658915 ) ) ;
#6958 = CYLINDRICAL_SURFACE ( 'NONE', #5545, 14.00000000000000178 ) ;
#6959 =( GEOMETRIC_REPRESENTATION_CONTEXT ( 3 ) GLOBAL_UNCERTAINTY_ASSIGNED_CONTEXT ( ( #8610 ) ) GLOBAL_UNIT_ASSIGNED_CONTEXT ( ( #13425, #2454, #9749 ) ) REPRESENTATION_CONTEXT ( 'NONE', 'WORKASPACE' ) );
#6960 = CARTESIAN_POINT ( 'NONE',  ( 26.12124691615246874, -10.79952268558355755, -14.20570119594951208 ) ) ;
#6961 = CARTESIAN_POINT ( 'NONE',  ( 24.63290760229943643, -10.17177306796459035, 14.56289668145355698 ) ) ;
#6962 = B_SPLINE_CURVE_WITH_KNOTS ( 'NONE', 3,
 ( #8001, #5446, #13717, #13540, #10873 ),
 .UNSPECIFIED., .F., .F.,
 ( 4, 1, 4 ),
 ( 0.000000000000000000, 0.002309401076758504923, 0.004618802153517009845 ),
 .UNSPECIFIED. ) ;
#6963 = FILL_AREA_STYLE_COLOUR ( '', #11281 ) ;
#6964 = CARTESIAN_POINT ( 'NONE',  ( 30.13703915187255689, -4.405930820630744371, -7.939653947423662039 ) ) ;
#6965 = ORIENTED_EDGE ( 'NONE', *, *, #6828, .T. ) ;
#6966 = CARTESIAN_POINT ( 'NONE',  ( 27.88665588685489993, -3.423116496867954162, -3.627061608673662008 ) ) ;
#6967 = AXIS2_PLACEMENT_3D ( 'NONE', #8203, #16542, #12093 ) ;
#6968 = CARTESIAN_POINT ( 'NONE',  ( 29.03376756790819613, -4.538853258604016006, -7.939653947423662039 ) ) ;
#6969 = VECTOR ( 'NONE', #16282, 1000.000000000000227 ) ;
#6970 = FACE_OUTER_BOUND ( 'NONE', #2864, .T. ) ;
#6971 = EDGE_CURVE ( 'NONE', #8875, #10810, #6926, .T. ) ;
#6972 = DIRECTION ( 'NONE',  ( -0.000000000000000000, -0.000000000000000000, -1.000000000000000000 ) ) ;
#6973 = ORIENTED_EDGE ( 'NONE', *, *, #7540, .F. ) ;
#6974 = ORIENTED_EDGE ( 'NONE', *, *, #7118, .T. ) ;
#6975 = CARTESIAN_POINT ( 'NONE',  ( 27.51889869220010354, -3.467423976192371526, 3.627061608673666449 ) ) ;
#6976 = EDGE_CURVE ( 'NONE', #14024, #9359, #11552, .T. ) ;
#6977 = CARTESIAN_POINT ( 'NONE',  ( 28.55151181693415907, -2.416235175459247486, -4.533357778048659803 ) ) ;
#6978 = CARTESIAN_POINT ( 'NONE',  ( 30.88568772756644520, -4.315733451902305617, 8.283357778048662468 ) ) ;
#6979 = CARTESIAN_POINT ( 'NONE',  ( -13.00000000000000178, 1.592040838891559293E-15, -12.00000000000000000 ) ) ;
#6980 = CARTESIAN_POINT ( 'NONE',  ( 28.63031693179632242, -2.406740715396564756, -4.533357778048659803 ) ) ;
#6981 = CARTESIAN_POINT ( 'NONE',  ( 27.73357241910951743, -6.576412695658750529, -6.861505862736166250 ) ) ;
#6982 = CARTESIAN_POINT ( 'NONE',  ( 29.84999239022537409, -5.894327871574777333, -3.283357778048667797 ) ) ;
#6983 = DIRECTION ( 'NONE',  ( 0.000000000000000000, -1.000000000000000000, -3.469446951953614189E-16 ) ) ;
#6984 = CIRCLE ( 'NONE', #15674, 2.000000000000001776 ) ;
#6985 = CARTESIAN_POINT ( 'NONE',  ( 28.16197717867739314, -7.161965777771100328, -5.113484796970856117 ) ) ;
#6986 = EDGE_CURVE ( 'NONE', #16315, #4277, #6569, .T. ) ;
#6987 = CARTESIAN_POINT ( 'NONE',  ( 29.54600080245929306, -4.477139269648729325, -3.283357778048664688 ) ) ;
#6988 = VECTOR ( 'NONE', #8403, 1000.000000000000227 ) ;
#6989 = CARTESIAN_POINT ( 'NONE',  ( 30.45225960443380231, -4.367952981209816343, -3.627061608673664672 ) ) ;
#6990 = CARTESIAN_POINT ( 'NONE',  ( 28.20260476654369697, -6.819712339336020612, -7.033357778048666908 ) ) ;
#6991 = DIRECTION ( 'NONE',  ( -0.000000000000000000, -0.000000000000000000, -1.000000000000000000 ) ) ;
#6992 = DIRECTION ( 'NONE',  ( -0.000000000000000000, -0.000000000000000000, -1.000000000000000000 ) ) ;
#6993 = DIRECTION ( 'NONE',  ( 0.7866107318554522720, -0.6174492339697490451, 8.659560562354985860E-17 ) ) ;
#6994 = CARTESIAN_POINT ( 'NONE',  ( 32.38298487551052318, -4.135338714860305132, 3.283357778048664244 ) ) ;
#6995 = CARTESIAN_POINT ( 'NONE',  ( 28.10549950023367316, -2.142809097641162897, -5.783357778048658915 ) ) ;
#6996 = VECTOR ( 'NONE', #1, 1000.000000000000000 ) ;
#6997 = AXIS2_PLACEMENT_3D ( 'NONE', #7328, #11464, #17030 ) ;
#6998 = ORIENTED_EDGE ( 'NONE', *, *, #9707, .T. ) ;
#6999 = CONICAL_SURFACE ( 'NONE', #15401, 2.041999999999999815, 1.047197551196591858 ) ;
#7000 = CARTESIAN_POINT ( 'NONE',  ( 32.32036211097666012, -1.624804527518282748, -5.783357778048663356 ) ) ;
#7001 = FACE_OUTER_BOUND ( 'NONE', #13560, .T. ) ;
#7002 = VECTOR ( 'NONE', #17343, 1000.000000000000114 ) ;
#7003 = VECTOR ( 'NONE', #1195, 1000.000000000000000 ) ;
#7004 = EDGE_LOOP ( 'NONE', ( #16078, #3646, #2320, #3138 ) ) ;
#7005 = CARTESIAN_POINT ( 'NONE',  ( -16.75000000000000000, -16.21813761408365195, -16.03574476417183448 ) ) ;
#7006 = ORIENTED_EDGE ( 'NONE', *, *, #3157, .F. ) ;
#7007 = CARTESIAN_POINT ( 'NONE',  ( 28.91547068018125799, -2.672194098943493135, -6.861505862736158257 ) ) ;
#7008 = ADVANCED_FACE ( 'NONE', ( #1074 ), #3801, .F. ) ;
#7009 = CARTESIAN_POINT ( 'NONE',  ( -0.3461262719736134530, 4.658553426539286946, -3.371615880910374674 ) ) ;
#7010 = ORIENTED_EDGE ( 'NONE', *, *, #8873, .T. ) ;
#7011 = ORIENTED_EDGE ( 'NONE', *, *, #4385, .T. ) ;
#7012 = CARTESIAN_POINT ( 'NONE',  ( 30.62726312072365431, -1.838986382273682718, -5.783357778048658027 ) ) ;
#7013 = CARTESIAN_POINT ( 'NONE',  ( -7.999999999999991118, -1.301042606982605321E-15, -4.700000000000000178 ) ) ;
#7014 = CARTESIAN_POINT ( 'NONE',  ( 0.000000000000000000, 0.000000000000000000, -3.000000000000002665 ) ) ;
#7015 = CIRCLE ( 'NONE', #5543, 0.9000000000000003553 ) ;
#7016 = CARTESIAN_POINT ( 'NONE',  ( 26.51200394741821498, -4.842675973971495296, -7.939653947423662039 ) ) ;
#7017 = AXIS2_PLACEMENT_3D ( 'NONE', #17650, #11798, #14721 ) ;
#7018 = ADVANCED_BREP_SHAPE_REPRESENTATION ( '', ( #11123, #3575 ), #15 ) ;
#7020 = EDGE_CURVE ( 'NONE', #10514, #9531, #13993, .T. ) ;
#7019 = ORIENTED_EDGE ( 'NONE', *, *, #2742, .T. ) ;
#7021 = LINE ( 'NONE', #12541, #5126 ) ;
#7022 = EDGE_CURVE ( 'NONE', #15625, #8115, #4717, .T. ) ;
#7023 = VERTEX_POINT ( 'NONE', #14858 ) ;
#7024 = CARTESIAN_POINT ( 'NONE',  ( 26.63392073224175505, -2.647267031729148012, 4.533357778048667797 ) ) ;
#7025 =( BOUNDED_CURVE ( )  B_SPLINE_CURVE ( 2, ( #7417, #436, #244, #5755, #15656, #11269, #3236, #8774, #14307 ),
 .UNSPECIFIED., .F., .T. ) 
 B_SPLINE_CURVE_WITH_KNOTS ( ( 3, 2, 2, 2, 3 ),
 ( 0.8653846153846154188, 0.8717948717948718063, 0.8846153846153845812, 0.8974358974358974672, 0.9012882778258578531 ),
 .UNSPECIFIED. ) 
 CURVE ( )  GEOMETRIC_REPRESENTATION_ITEM ( )  RATIONAL_B_SPLINE_CURVE ( ( 0.9330127018922192983, 0.9330127018922198534, 1.000000000000000000, 0.8660254037844387076, 1.000000000000000000, 0.8660254037844387076, 1.000000000000000000, 0.9597425536373320742, 0.9436786787937823107 ) ) 
 REPRESENTATION_ITEM ( '' )  );
#7026 = AXIS2_PLACEMENT_3D ( 'NONE', #17125, #151, #12929 ) ;
#7027 = CIRCLE ( 'NONE', #15426, 14.00000000000000178 ) ;
#7028 = CARTESIAN_POINT ( 'NONE',  ( 27.28266178881210280, -7.257709054644824853, 5.783357778048657138 ) ) ;
#7029 = CARTESIAN_POINT ( 'NONE',  ( -17.08586189024356727, -18.24992599651649527, 15.98693133205340189 ) ) ;
#7030 = LINE ( 'NONE', #12548, #5740 ) ;
#7031 = VERTEX_POINT ( 'NONE', #2185 ) ;
#7032 = VECTOR ( 'NONE', #17776, 1000.000000000000227 ) ;
#7033 = FILL_AREA_STYLE ('',( #4390 ) ) ;
#7034 = CARTESIAN_POINT ( 'NONE',  ( 8.250000000000014211, 6.495190528383269601, -3.000000000000000000 ) ) ;
#7035 = ADVANCED_FACE ( 'NONE', ( #3705 ), #14510, .F. ) ;
#7036 = ORIENTED_EDGE ( 'NONE', *, *, #16651, .T. ) ;
#7037 = CARTESIAN_POINT ( 'NONE',  ( -9.500000000000001776, 0.000000000000000000, -2.000000000000000000 ) ) ;
#7038 = EDGE_CURVE ( 'NONE', #15016, #9716, #14776, .T. ) ;
#7039 = CARTESIAN_POINT ( 'NONE',  ( 27.89118264539014547, -6.557423775948280742, -6.861505862736167138 ) ) ;
#7040 = CARTESIAN_POINT ( 'NONE',  ( 32.14656953781143756, -4.163822094218565972, -3.283357778048664688 ) ) ;
#7041 = CONICAL_SURFACE ( 'NONE', #16319, 9.500000000000001776, 0.7853981633974465026 ) ;
#7042 = DIRECTION ( 'NONE',  ( -1.000000000000000000, 0.000000000000000000, 0.000000000000000000 ) ) ;
#7043 = DIRECTION ( 'NONE',  ( 0.1080576791287503058, 0.9941446262900122122, 6.938893903907228378E-17 ) ) ;
#7044 = CARTESIAN_POINT ( 'NONE',  ( 33.76397967447234549, -5.422769698972272678, 3.283357778048663356 ) ) ;
#7045 = CARTESIAN_POINT ( 'NONE',  ( 30.04066231269008469, -3.163601260824890904, 3.627061608673666893 ) ) ;
#7046 = AXIS2_PLACEMENT_3D ( 'NONE', #6640, #847, #9443 ) ;
#7047 = FACE_OUTER_BOUND ( 'NONE', #4148, .T. ) ;
#7048 = DIRECTION ( 'NONE',  ( 0.000000000000000000, 0.000000000000000000, -1.000000000000000000 ) ) ;
#7049 = CARTESIAN_POINT ( 'NONE',  ( 28.39010325924584421, -2.735490497978389612, 6.861505862736166250 ) ) ;
#7050 = ORIENTED_EDGE ( 'NONE', *, *, #6280, .T. ) ;
#7051 = ORIENTED_EDGE ( 'NONE', *, *, #4540, .F. ) ;
#7052 = CARTESIAN_POINT ( 'NONE',  ( 28.56093688906631911, -4.595820017735426255, 7.939653947423662039 ) ) ;
#7053 = AXIS2_PLACEMENT_3D ( 'NONE', #1980, #5119, #13211 ) ;
#7054 = CARTESIAN_POINT ( 'NONE',  ( -50.00000000000000000, -16.03270077640482683, 5.537981825772250843 ) ) ;
#7055 = ORIENTED_EDGE ( 'NONE', *, *, #8588, .F. ) ;
#7056 = CARTESIAN_POINT ( 'NONE',  ( 30.69058026372202974, -5.793053633118939061, 3.283357778048663356 ) ) ;
#7057 = LINE ( 'NONE', #16851, #12120 ) ;
#7058 = DIRECTION ( 'NONE',  ( -1.000000000000000000, -0.000000000000000000, -0.000000000000000000 ) ) ;
#7059 = DIRECTION ( 'NONE',  ( 0.7020299829125996594, 0.08458074894285612377, 0.7071067811865480168 ) ) ;
#7060 = CARTESIAN_POINT ( 'NONE',  ( 27.45766530510195835, -4.728742455708699666, -3.627061608673664672 ) ) ;
#7061 = AXIS2_PLACEMENT_3D ( 'NONE', #16705, #12525, #10058 ) ;
#7062 = EDGE_CURVE ( 'NONE', #3307, #16117, #17393, .T. ) ;
#7063 = DIRECTION ( 'NONE',  ( -1.000000000000000000, 0.000000000000000000, -0.000000000000000000 ) ) ;
#7064 = ORIENTED_EDGE ( 'NONE', *, *, #14845, .T. ) ;
#7066 = EDGE_CURVE ( 'NONE', #4693, #15606, #4899, .T. ) ;
#7065 = CARTESIAN_POINT ( 'NONE',  ( 28.67914455963771303, -4.581578327848842669, -8.283357778048662468 ) ) ;
#7067 = CARTESIAN_POINT ( 'NONE',  ( 32.06776442294927421, -4.173316554281249147, -3.283357778048664688 ) ) ;
#7068 = CARTESIAN_POINT ( 'NONE',  ( 17.15697743806116549, -13.99005979112454767, -15.97644891051836957 ) ) ;
#7069 = DIRECTION ( 'NONE',  ( 0.000000000000000000, 0.000000000000000000, 1.000000000000000000 ) ) ;
#7070 = CARTESIAN_POINT ( 'NONE',  ( 32.51858583609114106, -1.611119345748072362, -5.783357778048658027 ) ) ;
#7071 = EDGE_CURVE ( 'NONE', #2203, #17907, #4876, .T. ) ;
#7072 = CARTESIAN_POINT ( 'NONE',  ( 28.91547068018125799, -2.672194098943493135, -6.861505862736158257 ) ) ;
#7073 = DIRECTION ( 'NONE',  ( -0.1196152422706621143, -0.9928203230275509661, 0.000000000000000000 ) ) ;
#7074 = VECTOR ( 'NONE', #3683, 1000.000000000000000 ) ;
#7075 = VERTEX_POINT ( 'NONE', #7788 ) ;
#7076 = VERTEX_POINT ( 'NONE', #5057 ) ;
#7077 = ORIENTED_EDGE ( 'NONE', *, *, #14445, .T. ) ;
#7078 = CARTESIAN_POINT ( 'NONE',  ( 29.36638131047866906, -1.990897739957422807, 5.783357778048668685 ) ) ;
#7079 = ORIENTED_EDGE ( 'NONE', *, *, #17232, .T. ) ;
#7080 = CARTESIAN_POINT ( 'NONE',  ( 33.76207435632690590, -3.969185667289998332, -3.627061608673664672 ) ) ;
#7081 = CARTESIAN_POINT ( 'NONE',  ( 25.78162057792670225, -2.952641328940847743, -4.882123357130833341 ) ) ;
#7082 = CARTESIAN_POINT ( 'NONE',  ( 33.78529456515154550, -6.484467084455914687, -5.783357778048663356 ) ) ;
#7083 = CARTESIAN_POINT ( 'NONE',  ( 29.60297508593253468, -5.724216059278466773, -7.939653947423664704 ) ) ;
#7084 = CARTESIAN_POINT ( 'NONE',  ( 26.85044460880409645, -7.319979551716484067, -5.783357778048668685 ) ) ;
#7085 = DIRECTION ( 'NONE',  ( -0.1196152422706610735, 0.9928203230275511881, 0.000000000000000000 ) ) ;
#7086 = EDGE_CURVE ( 'NONE', #15383, #12849, #10577, .T. ) ;
#7087 = CARTESIAN_POINT ( 'NONE',  ( 0.3208286057739613839, -4.433571671609690235, -0.3503314178412654245 ) ) ;
#7088 = CARTESIAN_POINT ( 'NONE',  ( 27.02423718196931546, -4.780961985016209503, -3.283357778048664688 ) ) ;
#7089 = ORIENTED_EDGE ( 'NONE', *, *, #13801, .F. ) ;
#7090 = CARTESIAN_POINT ( 'NONE',  ( 29.19137779418881351, -4.519864338893556877, -3.627061608673664672 ) ) ;
#7091 = CARTESIAN_POINT ( 'NONE',  ( -14.00000000000000178, 0.000000000000000000, -8.700000000000001066 ) ) ;
#7092 = DIRECTION ( 'NONE',  ( -1.000000000000000000, 0.000000000000000000, 0.000000000000000000 ) ) ;
#7093 = EDGE_CURVE ( 'NONE', #1236, #9636, #1731, .T. ) ;
#7094 = LINE ( 'NONE', #15425, #2561 ) ;
#7095 = CARTESIAN_POINT ( 'NONE',  ( 30.93441382992541477, -1.402235749049144609, 5.783357778048668685 ) ) ;
#7096 = CARTESIAN_POINT ( 'NONE',  ( 26.86653773853314320, -2.919050055179571945, -6.861505862736159145 ) ) ;
#7097 = AXIS2_PLACEMENT_3D ( 'NONE', #10961, #16523, #5269 ) ;
#7098 = ORIENTED_EDGE ( 'NONE', *, *, #9184, .F. ) ;
#7099 = ORIENTED_EDGE ( 'NONE', *, *, #11091, .F. ) ;
#7100 = VERTEX_POINT ( 'NONE', #8143 ) ;
#7101 = DIRECTION ( 'NONE',  ( 0.000000000000000000, 0.000000000000000000, -1.000000000000000000 ) ) ;
#7102 = CARTESIAN_POINT ( 'NONE',  ( 30.17644170758179101, -4.401183590806859947, -3.283357778048664688 ) ) ;
#7103 = B_SPLINE_CURVE_WITH_KNOTS ( 'NONE', 3,
 ( #7034, #11249, #11535, #10184 ),
 .UNSPECIFIED., .F., .F.,
 ( 4, 4 ),
 ( 2.843119637714455897E-07, 0.001422633878257845976 ),
 .UNSPECIFIED. ) ;
#7104 = DIRECTION ( 'NONE',  ( 0.1113444980252557837, -0.9937818688019538493, 0.000000000000000000 ) ) ;
#7105 = ORIENTED_EDGE ( 'NONE', *, *, #4484, .T. ) ;
#7106 = EDGE_CURVE ( 'NONE', #12046, #3520, #4158, .T. ) ;
#7107 = CARTESIAN_POINT ( 'NONE',  ( 30.60986983071443390, -4.348964061499348333, -3.627061608673664672 ) ) ;
#7108 = CARTESIAN_POINT ( 'NONE',  ( 27.55969062878875064, -7.234529412811931515, -5.783357778048668685 ) ) ;
#7109 = ORIENTED_EDGE ( 'NONE', *, *, #4720, .F. ) ;
#7110 = ORIENTED_EDGE ( 'NONE', *, *, #8996, .F. ) ;
#7111 = CARTESIAN_POINT ( 'NONE',  ( 29.82181869931131146, -4.443908660051686610, -3.627061608673664672 ) ) ;
#7112 = DIRECTION ( 'NONE',  ( -0.1196152422706611984, 0.9928203230275510771, 0.000000000000000000 ) ) ;
#7113 = DIRECTION ( 'NONE',  ( 1.000000000000000000, 0.000000000000000000, 0.000000000000000000 ) ) ;
#7114 = ORIENTED_EDGE ( 'NONE', *, *, #17743, .F. ) ;
#7115 = CARTESIAN_POINT ( 'NONE',  ( 31.07327543742414022, -2.112412460091767308, -4.533357778048659803 ) ) ;
#7116 = CARTESIAN_POINT ( 'NONE',  ( 17.07932405232147488, -18.26192153598439205, -15.98801167710370663 ) ) ;
#7117 = CARTESIAN_POINT ( 'NONE',  ( 32.67202617590239555, -5.981426544730773287, 6.861505862736158257 ) ) ;
#7118 = EDGE_CURVE ( 'NONE', #11071, #17243, #9655, .T. ) ;
#7119 = CARTESIAN_POINT ( 'NONE',  ( 26.60838078660069428, -6.085005533777348319, 3.627061608673662896 ) ) ;
#7120 = CARTESIAN_POINT ( 'NONE',  ( -27.94765010173961883, -20.05889348609997924, 13.73347386810006832 ) ) ;
#7121 = DIRECTION ( 'NONE',  ( -0.1196152422706611151, 0.9928203230275511881, 0.000000000000000000 ) ) ;
#7122 = ORIENTED_EDGE ( 'NONE', *, *, #2538, .T. ) ;
#7123 = CARTESIAN_POINT ( 'NONE',  ( 26.28639176851562453, -7.142300497639897827, -6.903997060601237301 ) ) ;
#7124 = VERTEX_POINT ( 'NONE', #11099 ) ;
#7125 = CARTESIAN_POINT ( 'NONE',  ( 26.95740407890011170, -7.307093047852763590, 5.113484796970857005 ) ) ;
#7126 = ADVANCED_FACE ( 'NONE', ( #157 ), #5670, .T. ) ;
#7127 = EDGE_LOOP ( 'NONE', ( #5373, #554, #9221 ) ) ;
#7128 = FACE_OUTER_BOUND ( 'NONE', #12946, .T. ) ;
#7129 = CARTESIAN_POINT ( 'NONE',  ( 28.28955653359400557, -5.882457056865704637, -3.627061608673668225 ) ) ;
#7130 = CARTESIAN_POINT ( 'NONE',  ( 31.92138306490751987, -2.737139032229836122, -3.283357778048662023 ) ) ;
#7131 = CARTESIAN_POINT ( 'NONE',  ( -5.499998387031001634, -20.49508120620799900, 6.000000000000000000 ) ) ;
#7132 = DIRECTION ( 'NONE',  ( -0.000000000000000000, -0.000000000000000000, -1.000000000000000000 ) ) ;
#7133 =( BOUNDED_CURVE ( )  B_SPLINE_CURVE ( 2, ( #7497, #10378, #13020, #7855, #15932, #3503, #9035, #2163, #6403 ),
 .UNSPECIFIED., .F., .T. ) 
 B_SPLINE_CURVE_WITH_KNOTS ( ( 3, 2, 2, 2, 3 ),
 ( 0.7884615384615384359, 0.7948717948717948234, 0.8076923076923077094, 0.8205128205128204844, 0.8269230769230769829 ),
 .UNSPECIFIED. ) 
 CURVE ( )  GEOMETRIC_REPRESENTATION_ITEM ( )  RATIONAL_B_SPLINE_CURVE ( ( 0.9330127018922194093, 0.9330127018922194093, 1.000000000000000000, 0.8660254037844387076, 1.000000000000000000, 0.8660254037844387076, 1.000000000000000000, 0.9330127018922187432, 0.9330127018922192983 ) ) 
 REPRESENTATION_ITEM ( '' )  );
#7134 = CARTESIAN_POINT ( 'NONE',  ( 32.93832978346670615, -1.887710243310447567, -7.033357778048658027 ) ) ;
#7135 = DIRECTION ( 'NONE',  ( 0.000000000000000000, 0.000000000000000000, 1.000000000000000000 ) ) ;
#7136 = CARTESIAN_POINT ( 'NONE',  ( -15.92260893619738837, -28.39189527176317540, -16.15082599432113142 ) ) ;
#7137 = CARTESIAN_POINT ( 'NONE',  ( 29.97942892559193950, -4.424919740341219487, 7.939653947423662039 ) ) ;
#7138 = EDGE_CURVE ( 'NONE', #2767, #7075, #2296, .T. ) ;
#7139 = ORIENTED_EDGE ( 'NONE', *, *, #11950, .T. ) ;
#7140 = ADVANCED_FACE ( 'NONE', ( #10839 ), #9487, .F. ) ;
#7141 = ORIENTED_EDGE ( 'NONE', *, *, #15038, .F. ) ;
#7142 = CARTESIAN_POINT ( 'NONE',  ( 28.99445422935450267, -6.424501337975009996, 4.705209693361160461 ) ) ;
#7143 = LINE ( 'NONE', #3056, #15399 ) ;
#7144 = CARTESIAN_POINT ( 'NONE',  ( 34.51156627690993162, -8.531090163810741700, -5.783357778048662468 ) ) ;
#7145 = ORIENTED_EDGE ( 'NONE', *, *, #13786, .F. ) ;
#7146 = CARTESIAN_POINT ( 'NONE',  ( 27.26074174026764751, -6.633379454790151009, 4.705209693361159573 ) ) ;
#7147 = DIRECTION ( 'NONE',  ( 0.9928203230275512992, 0.1196152422706610180, 4.006172263299093133E-17 ) ) ;
#7148 = ORIENTED_EDGE ( 'NONE', *, *, #17475, .T. ) ;
#7149 = CARTESIAN_POINT ( 'NONE',  ( -4.000000000000000000, 1.700072946616194569, -3.020308295356459727 ) ) ;
#7150 = CARTESIAN_POINT ( 'NONE',  ( 4.211140560182196957, 2.431303136016537803, -3.445885042887434579 ) ) ;
#7151 = CARTESIAN_POINT ( 'NONE',  ( 26.56758885001203652, -2.317900097157796324, -5.783357778048670461 ) ) ;
#7152 = ORIENTED_EDGE ( 'NONE', *, *, #3627, .F. ) ;
#7153 = CARTESIAN_POINT ( 'NONE',  ( 29.46348657678868577, -6.667800981652280967, -7.033357778048666908 ) ) ;
#7154 = FACE_OUTER_BOUND ( 'NONE', #473, .T. ) ;
#7155 = DIRECTION ( 'NONE',  ( 0.000000000000000000, 0.000000000000000000, 1.000000000000000000 ) ) ;
#7156 =( NAMED_UNIT ( * ) PLANE_ANGLE_UNIT ( ) SI_UNIT ( $, .RADIAN. ) );
#7157 = CARTESIAN_POINT ( 'NONE',  ( 31.88814493096863956, -1.687075024589942851, -5.783357778048658027 ) ) ;
#7158 = VERTEX_POINT ( 'NONE', #13933 ) ;
#7159 =( BOUNDED_CURVE ( )  B_SPLINE_CURVE ( 2, ( #11498, #9138, #5888, #14341, #7447, #3176, #11411, #1737, #12022 ),
 .UNSPECIFIED., .F., .T. ) 
 B_SPLINE_CURVE_WITH_KNOTS ( ( 3, 2, 2, 2, 3 ),
 ( 0.05769230769230770939, 0.06410256410256409687, 0.07692307692307692735, 0.08974358974358974395, 0.09615384615384617306 ),
 .UNSPECIFIED. ) 
 CURVE ( )  GEOMETRIC_REPRESENTATION_ITEM ( )  RATIONAL_B_SPLINE_CURVE ( ( 0.9330127018922194093, 0.9330127018922196314, 1.000000000000000000, 0.8660254037844387076, 1.000000000000000000, 0.8660254037844387076, 1.000000000000000000, 0.9330127018922191873, 0.9330127018922194093 ) ) 
 REPRESENTATION_ITEM ( '' )  );
#7160 = CARTESIAN_POINT ( 'NONE',  ( 27.26074174026764751, -6.633379454790151009, -6.861505862736167138 ) ) ;
#7161 = DIRECTION ( 'NONE',  ( -1.000000000000000000, 0.000000000000000000, 0.000000000000000000 ) ) ;
#7162 = ADVANCED_FACE ( 'NONE', ( #6779 ), #5400, .F. ) ;
#7163 = ORIENTED_EDGE ( 'NONE', *, *, #1880, .T. ) ;
#7164 = CIRCLE ( 'NONE', #13527, 2.500000000000001776 ) ;
#7165 = ADVANCED_FACE ( 'NONE', ( #6952 ), #1427, .F. ) ;
#7166 = EDGE_LOOP ( 'NONE', ( #16377, #2177, #9802, #5450 ) ) ;
#7167 = CARTESIAN_POINT ( 'NONE',  ( 27.73357241910951743, -6.576412695658750529, 4.705209693361160461 ) ) ;
#7168 = B_SPLINE_CURVE_WITH_KNOTS ( 'NONE', 3,
 ( #7633, #3279, #17352, #2013, #10419, #14343, #13062, #11966 ),
 .UNSPECIFIED., .F., .F.,
 ( 4, 2, 2, 4 ),
 ( 2.465131517101105978E-07, 0.001183067374689841323, 0.001774477805458907036, 0.002365888236227972966 ),
 .UNSPECIFIED. ) ;
#7169 = CARTESIAN_POINT ( 'NONE',  ( 26.36761712467744090, -6.740983333149474177, -4.705209693361168455 ) ) ;
#7170 = CARTESIAN_POINT ( 'NONE',  ( 5.000000000000002665, 3.306546357697854226E-16, 2.700000000000000622 ) ) ;
#7171 = VECTOR ( 'NONE', #11339, 1000.000000000000114 ) ;
#7172 = FACE_BOUND ( 'NONE', #13603, .T. ) ;
#7173 = CARTESIAN_POINT ( 'NONE',  ( 29.01637427789896151, -7.048830937829683840, -5.783357778048668685 ) ) ;
#7174 = CARTESIAN_POINT ( 'NONE',  ( 29.39961944441754227, -3.040961747597316744, -3.283357778048662023 ) ) ;
#7175 = EDGE_CURVE ( 'NONE', #12037, #9975, #5187, .T. ) ;
#7176 = DIRECTION ( 'NONE',  ( -1.000000000000000000, 0.000000000000000000, 0.000000000000000000 ) ) ;
#7177 = CARTESIAN_POINT ( 'NONE',  ( 12.50000000000000000, 1.530808498934191521E-15, -12.00000000000000000 ) ) ;
#7178 = UNCERTAINTY_MEASURE_WITH_UNIT (LENGTH_MEASURE( 1.000000000000000082E-05 ), #10875, 'distance_accuracy_value', 'NONE');
#7179 = LINE ( 'NONE', #12687, #12831 ) ;
#7180 = CARTESIAN_POINT ( 'NONE',  ( 28.99445422935450267, -6.424501337975009996, -6.861505862736166250 ) ) ;
#7181 = CARTESIAN_POINT ( 'NONE',  ( 4.281152949374508410, -4.203775615332241422, -3.000000000000000888 ) ) ;
#7182 = CARTESIAN_POINT ( 'NONE',  ( 23.00000000000000000, -16.21813761408365195, 13.00000000000000178 ) ) ;
#7183 = CARTESIAN_POINT ( 'NONE',  ( 26.06962060539356330, -5.343074812781621219, -3.590724507760069795 ) ) ;
#7184 = DIRECTION ( 'NONE',  ( 0.9928203230275512992, 0.1196152422706607682, -0.000000000000000000 ) ) ;
#7185 = AXIS2_PLACEMENT_3D ( 'NONE', #1308, #10884, #9705 ) ;
#7186 = CARTESIAN_POINT ( 'NONE',  ( 32.85952466860454280, -1.897204703373130741, 4.533357778048667797 ) ) ;
#7187 = CARTESIAN_POINT ( 'NONE',  ( 26.24062359194589433, -6.129313013101782559, -3.627061608673667781 ) ) ;
#7188 = EDGE_CURVE ( 'NONE', #7756, #3522, #12577, .T. ) ;
#7189 = VERTEX_POINT ( 'NONE', #16573 ) ;
#7190 = CARTESIAN_POINT ( 'NONE',  ( 26.01652455409633902, -4.902371455920926380, -5.783357778048663356 ) ) ;
#7191 = CARTESIAN_POINT ( 'NONE',  ( 46.98536657994561949, -3.383271691264599035, -5.783357778048662468 ) ) ;
#7192 = DIRECTION ( 'NONE',  ( 1.000000000000000000, 0.000000000000000000, 0.000000000000000000 ) ) ;
#7193 = ORIENTED_EDGE ( 'NONE', *, *, #13165, .T. ) ;
#7194 = ADVANCED_FACE ( 'NONE', ( #14944 ), #8048, .T. ) ;
#7195 = AXIS2_PLACEMENT_3D ( 'NONE', #995, #3436, #3703 ) ;
#7196 = CARTESIAN_POINT ( 'NONE',  ( 26.49878054387835746, -2.963357534503999968, -4.705209693361160461 ) ) ;
#7197 = ORIENTED_EDGE ( 'NONE', *, *, #10518, .T. ) ;
#7198 = CARTESIAN_POINT ( 'NONE',  ( 30.27725608814395031, -6.896919580145944195, -5.783357778048668685 ) ) ;
#7199 = CARTESIAN_POINT ( 'NONE',  ( -36.27615609941022257, -23.17738945083361202, 11.07596365154449636 ) ) ;
#7200 = CARTESIAN_POINT ( 'NONE',  ( 30.08145424927873535, -6.930706697444451336, -5.783357778048663356 ) ) ;
#7201 = ORIENTED_EDGE ( 'NONE', *, *, #6767, .T. ) ;
#7202 = AXIS2_PLACEMENT_3D ( 'NONE', #5417, #17808, #5070 ) ;
#7203 = CARTESIAN_POINT ( 'NONE',  ( 30.93441382992541477, -1.402235749049144609, -5.783357778048658027 ) ) ;
#7204 = DIRECTION ( 'NONE',  ( 0.000000000000000000, 0.000000000000000000, 1.000000000000000000 ) ) ;
#7205 = ORIENTED_EDGE ( 'NONE', *, *, #12952, .F. ) ;
#7206 = CARTESIAN_POINT ( 'NONE',  ( 32.97402322492378346, -4.064130265842336165, 7.939653947423662039 ) ) ;
#7207 = AXIS2_PLACEMENT_3D ( 'NONE', #12658, #69, #2873 ) ;
#7208 = AXIS2_PLACEMENT_3D ( 'NONE', #1738, #5975, #11499 ) ;
#7209 = CARTESIAN_POINT ( 'NONE',  ( 25.93489015466116854, -5.606035894254070229, 3.627061608673662896 ) ) ;
#7210 = CARTESIAN_POINT ( 'NONE',  ( 29.32081432955537537, -3.050456207659999475, 8.283357778048666020 ) ) ;
#7211 = ORIENTED_EDGE ( 'NONE', *, *, #2485, .T. ) ;
#7212 = CARTESIAN_POINT ( 'NONE',  ( 28.82057243903374655, -7.082618055128190093, 5.783357778048657138 ) ) ;
#7213 = ORIENTED_EDGE ( 'NONE', *, *, #7589, .T. ) ;
#7214 = DIRECTION ( 'NONE',  ( -1.000000000000000000, -1.224646799147353454E-16, 0.000000000000000000 ) ) ;
#7215 = EDGE_LOOP ( 'NONE', ( #5610, #8542, #14504, #7712 ) ) ;
#7216 = DIRECTION ( 'NONE',  ( 0.000000000000000000, 0.000000000000000000, 1.000000000000000000 ) ) ;
#7217 = CARTESIAN_POINT ( 'NONE',  ( 33.69269431359690969, -6.158264969628857166, -4.533357778048668685 ) ) ;
#7218 = CIRCLE ( 'NONE', #14156, 6.249999999999996447 ) ;
#7219 = ADVANCED_FACE ( 'NONE', ( #16405 ), #15036, .F. ) ;
#7220 = CARTESIAN_POINT ( 'NONE',  ( 31.51612863268893960, -4.239777773060436239, -3.283357778048664688 ) ) ;
#7221 = CARTESIAN_POINT ( 'NONE',  ( -3.999999999999998224, 0.000000000000000000, 0.000000000000000000 ) ) ;
#7222 = DIRECTION ( 'NONE',  ( 1.000000000000000000, 0.000000000000000000, 0.000000000000000000 ) ) ;
#7223 = CARTESIAN_POINT ( 'NONE',  ( 32.70264286945147347, -5.350767304972614546, -3.627061608673668225 ) ) ;
#7224 = PLANE ( 'NONE',  #13964 ) ;
#7225 = CARTESIAN_POINT ( 'NONE',  ( 30.45719375084302527, -1.849279520242854469, -5.113484796970851676 ) ) ;
#7226 = CARTESIAN_POINT ( 'NONE',  ( 29.02054416436834217, -2.659534819136519790, 6.861505862736166250 ) ) ;
#7227 = ORIENTED_EDGE ( 'NONE', *, *, #9942, .T. ) ;
#7228 = AXIS2_PLACEMENT_3D ( 'NONE', #12033, #3887, #16230 ) ;
#7229 = VERTEX_POINT ( 'NONE', #16485 ) ;
#7230 = CARTESIAN_POINT ( 'NONE',  ( 28.12741954877813555, -2.767138697495831856, 4.705209693361167567 ) ) ;
#7231 = CYLINDRICAL_SURFACE ( 'NONE', #15687, 2.500000000000001776 ) ;
#7232 = LINE ( 'NONE', #7054, #15408 ) ;
#7233 = ORIENTED_EDGE ( 'NONE', *, *, #3217, .F. ) ;
#7234 = CARTESIAN_POINT ( 'NONE',  ( 27.77288575766320378, -4.690764616287755651, 3.627061608673664228 ) ) ;
#7235 = FACE_OUTER_BOUND ( 'NONE', #1187, .T. ) ;
#7236 = CARTESIAN_POINT ( 'NONE',  ( 0.000000000000000000, 0.000000000000000000, 2.399999999999999467 ) ) ;
#7237 = FACE_OUTER_BOUND ( 'NONE', #2221, .T. ) ;
#7238 = CARTESIAN_POINT ( 'NONE',  ( 39.47566789204768867, -7.933013952457433682, -5.783357778048662468 ) ) ;
#7239 = CARTESIAN_POINT ( 'NONE',  ( 27.24942365487322959, -6.207645047004940686, -3.283357778048667797 ) ) ;
#7240 =( BOUNDED_SURFACE ( )  B_SPLINE_SURFACE ( 3, 2, ( 
 ( #13168, #7816, #10430 ),
 ( #13346, #8995, #3730 ),
 ( #926, #9254, #9342 ),
 ( #17644, #5165, #10681 ),
 ( #7644, #1018, #2390 ),
 ( #16256, #17369, #658 ) ),
 .UNSPECIFIED., .F., .F., .T. ) 
 B_SPLINE_SURFACE_WITH_KNOTS ( ( 4, 2, 4 ),
 ( 3, 3 ),
 ( 0.02023740217035201183, 0.02269762987400600340, 0.02515785757765999150 ),
 ( 0.000000000000000000, 1.000000000000000000 ),
 .UNSPECIFIED. ) 
 GEOMETRIC_REPRESENTATION_ITEM ( )  RATIONAL_B_SPLINE_SURFACE ( (
 ( 1.000000000000000000, 0.8047781539129728046, 1.000000000000000000),
 ( 1.000000000000000000, 0.8123770319058200018, 1.000000000000000000),
 ( 1.000000000000000000, 0.8190663783055447400, 1.000000000000000000),
 ( 1.000000000000000000, 0.8192359702878471150, 1.000000000000000000),
 ( 1.000000000000000000, 0.8126134888418757862, 1.000000000000000000),
 ( 1.000000000000000000, 0.8047712368238109093, 1.000000000000000000) ) ) 
 REPRESENTATION_ITEM ( '' )  SURFACE ( )  );
#7241 = CARTESIAN_POINT ( 'NONE',  ( 27.46709037723411839, -6.908327297984874882, -4.533357778048668685 ) ) ;
#7242 = ADVANCED_FACE ( 'NONE', ( #9568 ), #15026, .T. ) ;
#7243 = CARTESIAN_POINT ( 'NONE',  ( 10.27627944162883544, 4.200961894323318013, -11.72793873352922489 ) ) ;
#7244 = CARTESIAN_POINT ( 'NONE',  ( 2.500000000000000000, 0.000000000000000000, 0.000000000000000000 ) ) ;
#7245 = CARTESIAN_POINT ( 'NONE',  ( 30.45225960443380231, -4.367952981209816343, -3.627061608673664672 ) ) ;
#7246 = AXIS2_PLACEMENT_3D ( 'NONE', #6577, #9129, #10292 ) ;
#7247 = CARTESIAN_POINT ( 'NONE',  ( 25.96814307759224150, -4.500799614243312874, -8.119953194407841579 ) ) ;
#7248 = DIRECTION ( 'NONE',  ( 0.9928203230275512992, 0.1196152422706614482, 0.000000000000000000 ) ) ;
#7249 = ADVANCED_BREP_SHAPE_REPRESENTATION ( '', ( #5349, #3575 ), #4782 ) ;
#7250 = ORIENTED_EDGE ( 'NONE', *, *, #2538, .F. ) ;
#7251 = ORIENTED_EDGE ( 'NONE', *, *, #11689, .T. ) ;
#7252 = EDGE_LOOP ( 'NONE', ( #6532, #3699, #300, #1694 ) ) ;
#7253 = CARTESIAN_POINT ( 'NONE',  ( 28.23249303296521617, -2.754479417688857179, 6.861505862736165362 ) ) ;
#7254 = CARTESIAN_POINT ( 'NONE',  ( 33.68326924318660076, -3.978680127145231893, -3.283357778048664688 ) ) ;
#7255 = DIRECTION ( 'NONE',  ( -1.000000000000000000, 0.000000000000000000, 0.000000000000000000 ) ) ;
#7256 = CARTESIAN_POINT ( 'NONE',  ( 4.000000000000000000, 2.309401076758498483, -4.700000000000000178 ) ) ;
#7257 = CARTESIAN_POINT ( 'NONE',  ( -2.016448651773435938E-27, -20.49999999999999645, -6.000000000000000000 ) ) ;
#7258 = CARTESIAN_POINT ( 'NONE',  ( 33.32855701603872234, -2.140504347050403045, -6.861505862736158257 ) ) ;
#7259 = CARTESIAN_POINT ( 'NONE',  ( 31.08763465596552322, -1.773323841400983758, -5.113484796970854340 ) ) ;
#7260 = DIRECTION ( 'NONE',  ( 0.7999999999999999334, 0.6000000000000000888, 0.000000000000000000 ) ) ;
#7261 = FACE_OUTER_BOUND ( 'NONE', #11043, .T. ) ;
#7262 =( BOUNDED_CURVE ( )  B_SPLINE_CURVE ( 2, ( #5671, #2707, #8583, #4326, #11012, #14118, #9569, #4417, #8498 ),
 .UNSPECIFIED., .F., .T. ) 
 B_SPLINE_CURVE_WITH_KNOTS ( ( 3, 2, 2, 2, 3 ),
 ( 0.01923076923076924918, 0.02564102564102564014, 0.03846153846153846367, 0.05128205128205128027, 0.05769230769230770939 ),
 .UNSPECIFIED. ) 
 CURVE ( )  GEOMETRIC_REPRESENTATION_ITEM ( )  RATIONAL_B_SPLINE_CURVE ( ( 0.9330127018922194093, 0.9330127018922195203, 1.000000000000000000, 0.8660254037844387076, 1.000000000000000000, 0.8660254037844387076, 1.000000000000000000, 0.9330127018922191873, 0.9330127018922194093 ) ) 
 REPRESENTATION_ITEM ( '' )  );
#7263 = EDGE_CURVE ( 'NONE', #2089, #1570, #16493, .T. ) ;
#7264 = CARTESIAN_POINT ( 'NONE',  ( 28.11132641904908169, -7.168068194032743534, -5.783357778048668685 ) ) ;
#7265 = EDGE_CURVE ( 'NONE', #6202, #2263, #12575, .T. ) ;
#7266 = AXIS2_PLACEMENT_3D ( 'NONE', #7604, #17609, #2083 ) ;
#7267 = CARTESIAN_POINT ( 'NONE',  ( 28.86293393808771057, -2.678523738846987357, -4.705209693361161349 ) ) ;
#7268 = CARTESIAN_POINT ( 'NONE',  ( -1.500000000000000000, 11.00000000000000000, -9.708203932499369415 ) ) ;
#7269 = CARTESIAN_POINT ( 'NONE',  ( 32.24155699611449677, -1.634298987580965923, -5.783357778048664244 ) ) ;
#7270 = CARTESIAN_POINT ( 'NONE',  ( -2.016448651773435938E-27, -20.49999999999999645, 13.00000000000000178 ) ) ;
#7271 = CARTESIAN_POINT ( 'NONE',  ( 26.61898274975073164, -6.283600725846810953, 8.283357778048660691 ) ) ;
#7272 = AXIS2_PLACEMENT_3D ( 'NONE', #6160, #15779, #14239 ) ;
#7273 = COLOUR_RGB ( '', 0.72549020, 0.75294118, 0.79215686) ;
#7274 = CARTESIAN_POINT ( 'NONE',  ( 28.41265020943543362, -1.706058464416624787, 5.783357778048668685 ) ) ;
#7275 = CARTESIAN_POINT ( 'NONE',  ( 26.01652455409633902, -4.902371455920926380, 5.783357778048663356 ) ) ;
#7276 = ORIENTED_EDGE ( 'NONE', *, *, #11915, .F. ) ;
#7277 = CIRCLE ( 'NONE', #11606, 5.000000000000000000 ) ;
#7278 = AXIS2_PLACEMENT_3D ( 'NONE', #1065, #9647, #9728 ) ;
#7279 = CARTESIAN_POINT ( 'NONE',  ( 0.000000000000000000, 0.000000000000000000, -4.000000000000000000 ) ) ;
#7280 = DIRECTION ( 'NONE',  ( -0.000000000000000000, -0.000000000000000000, 1.000000000000000000 ) ) ;
#7281 = CARTESIAN_POINT ( 'NONE',  ( -18.05564684537134568, -12.37312016356480449, -15.83930707548887895 ) ) ;
#7282 = ORIENTED_EDGE ( 'NONE', *, *, #13895, .T. ) ;
#7283 = AXIS2_PLACEMENT_3D ( 'NONE', #13763, #6863, #12394 ) ;
#7284 = DIRECTION ( 'NONE',  ( 0.1196152422706618645, -0.9928203230275510771, 0.000000000000000000 ) ) ;
#7285 = EDGE_CURVE ( 'NONE', #14407, #8284, #8860, .T. ) ;
#7286 = CARTESIAN_POINT ( 'NONE',  ( 30.90769699326644826, -6.820963901304073929, -5.783357778048668685 ) ) ;
#7287 = ORIENTED_EDGE ( 'NONE', *, *, #27, .T. ) ;
#7288 = DIRECTION ( 'NONE',  ( 1.000000000000000000, 0.000000000000000000, 0.000000000000000000 ) ) ;
#7289 = DIRECTION ( 'NONE',  ( 0.1196152422706609625, -0.9928203230275510771, -0.000000000000000000 ) ) ;
#7290 = DIRECTION ( 'NONE',  ( -0.000000000000000000, -0.000000000000000000, 1.000000000000000000 ) ) ;
#7291 = CARTESIAN_POINT ( 'NONE',  ( 30.80688261270428541, -4.325227911964988792, -3.283357778048664688 ) ) ;
#7292 = CARTESIAN_POINT ( 'NONE',  ( 31.87265695910486230, -5.650636735497883478, -8.283357778048664244 ) ) ;
#7293 = EDGE_CURVE ( 'NONE', #4903, #7100, #15945, .T. ) ;
#7294 = ORIENTED_EDGE ( 'NONE', *, *, #8798, .T. ) ;
#7295 = CARTESIAN_POINT ( 'NONE',  ( 26.47260139170898441, -4.847423203795396596, 8.283357778048662468 ) ) ;
#7296 = AXIS2_PLACEMENT_3D ( 'NONE', #4444, #15593, #3171 ) ;
#7297 = CARTESIAN_POINT ( 'NONE',  ( 30.40088504037531791, -1.856063607844930852, -6.453230759126464378 ) ) ;
#7298 = CARTESIAN_POINT ( 'NONE',  ( -17.70832741558421830, -19.55032950225749389, 15.89323616604937328 ) ) ;
#7299 = FACE_OUTER_BOUND ( 'NONE', #2646, .T. ) ;
#7300 = AXIS2_PLACEMENT_3D ( 'NONE', #9931, #1428, #15481 ) ;
#7301 = VERTEX_POINT ( 'NONE', #1803 ) ;
#7302 = CARTESIAN_POINT ( 'NONE',  ( -8.632250723006722026, -18.84644399697197770, 16.84735068286508763 ) ) ;
#7303 = VERTEX_POINT ( 'NONE', #1705 ) ;
#7304 = CARTESIAN_POINT ( 'NONE',  ( 0.000000000000000000, 0.000000000000000000, 1.102182119232618281E-16 ) ) ;
#7305 = DIRECTION ( 'NONE',  ( 0.6000000000000001998, 0.7999999999999999334, 0.000000000000000000 ) ) ;
#7306 = ORIENTED_EDGE ( 'NONE', *, *, #10158, .F. ) ;
#7307 = CARTESIAN_POINT ( 'NONE',  ( 26.92924972366625980, -7.310485091653801781, -5.783357778048657138 ) ) ;
#7308 = CARTESIAN_POINT ( 'NONE',  ( 26.37178701114681800, -2.351687214456304353, -5.783357778048658027 ) ) ;
#7309 = CIRCLE ( 'NONE', #4102, 11.29999999999999893 ) ;
#7310 = VECTOR ( 'NONE', #15321, 1000.000000000000227 ) ;
#7311 = ADVANCED_FACE ( 'NONE', ( #4503 ), #187, .F. ) ;
#7312 = CARTESIAN_POINT ( 'NONE',  ( 31.24973580796908834, -6.452593224933654170, -4.533357778048668685 ) ) ;
#7313 = CARTESIAN_POINT ( 'NONE',  ( -4.000000000000000000, 1.941961291383474508, -0.3515519931180230984 ) ) ;
#7314 = APPLICATION_PROTOCOL_DEFINITION ( 'draft international standard', 'automotive_design', 1998, #13956 ) ;
#7315 = CARTESIAN_POINT ( 'NONE',  ( 2.500000000000000000, -2.357898499370431722, 2.818925648462311528E-15 ) ) ;
#7316 = CARTESIAN_POINT ( 'NONE',  ( 27.75966235412334981, -2.811446176820259879, -4.705209693361160461 ) ) ;
#7317 = CARTESIAN_POINT ( 'NONE',  ( -4.211140560182196957, -2.431303136016548017, -3.445885042887436356 ) ) ;
#7318 = DIRECTION ( 'NONE',  ( -0.000000000000000000, -0.000000000000000000, -1.000000000000000000 ) ) ;
#7319 = CARTESIAN_POINT ( 'NONE',  ( 29.14000323013032556, -2.007974965528672495, 5.113484796970859669 ) ) ;
#7320 = ADVANCED_FACE ( 'NONE', ( #12751 ), #12850, .F. ) ;
#7321 = CARTESIAN_POINT ( 'NONE',  ( 29.04699097144805364, -6.418171698071525100, 6.861505862736157368 ) ) ;
#7322 = ORIENTED_EDGE ( 'NONE', *, *, #10507, .F. ) ;
#7323 = AXIS2_PLACEMENT_3D ( 'NONE', #8179, #13619, #4094 ) ;
#7324 = CARTESIAN_POINT ( 'NONE',  ( 25.41044654184514329, -5.982623484807521486, 5.783357778048662468 ) ) ;
#7325 = EDGE_LOOP ( 'NONE', ( #3031, #16020, #13238, #2024 ) ) ;
#7326 = EDGE_CURVE ( 'NONE', #13340, #8791, #16234, .T. ) ;
#7327 = CARTESIAN_POINT ( 'NONE',  ( 28.13194630731337753, -5.901445976576171759, 7.939653947423658487 ) ) ;
#7328 = CARTESIAN_POINT ( 'NONE',  ( -2.016448651773435938E-27, -20.49999999999999645, 13.00000000000000178 ) ) ;
#7329 = CARTESIAN_POINT ( 'NONE',  ( -2.016448651773435938E-27, -20.49999999999999645, -13.00000000000000178 ) ) ;
#7330 = ORIENTED_EDGE ( 'NONE', *, *, #7138, .T. ) ;
#7331 = CARTESIAN_POINT ( 'NONE',  ( 28.52162355051263987, -6.481468097106410475, 4.705209693361159573 ) ) ;
#7332 = ORIENTED_EDGE ( 'NONE', *, *, #3556, .F. ) ;
#7333 = CARTESIAN_POINT ( 'NONE',  ( -4.000000000000000000, -2.472261030551091476, -3.387027369136294208 ) ) ;
#7334 = ORIENTED_EDGE ( 'NONE', *, *, #16942, .F. ) ;
#7335 = CARTESIAN_POINT ( 'NONE',  ( -20.25000000000000711, -16.21813761408365195, -13.00000000000000178 ) ) ;
#7336 = DIRECTION ( 'NONE',  ( 0.9928203230275511881, 0.1196152422706610735, 9.614813431917827710E-17 ) ) ;
#7337 = CARTESIAN_POINT ( 'NONE',  ( 25.90934487712385348, 0.1208734971681838660, 5.783357778048663356 ) ) ;
#7338 = CARTESIAN_POINT ( 'NONE',  ( 28.23639288985533824, -7.542548330185622874, -5.783357778048669573 ) ) ;
#7339 = CARTESIAN_POINT ( 'NONE',  ( 33.68326924318660076, -3.978680127145231893, -3.283357778048664688 ) ) ;
#7340 = LINE ( 'NONE', #355, #9256 ) ;
#7341 = VECTOR ( 'NONE', #17578, 1000.000000000000000 ) ;
#7342 = CARTESIAN_POINT ( 'NONE',  ( 29.99682221560115991, -1.914942061115552541, -5.783357778048658027 ) ) ;
#7343 = ORIENTED_EDGE ( 'NONE', *, *, #17406, .T. ) ;
#7344 = AXIS2_PLACEMENT_3D ( 'NONE', #4930, #3595, #9117 ) ;
#7345 = CARTESIAN_POINT ( 'NONE',  ( 28.79241808379989465, -7.086010098929231837, 6.453230759126462601 ) ) ;
#7346 = CARTESIAN_POINT ( 'NONE',  ( 35.62429925076629189, -17.76690233603958902, -0.5379818257722508434 ) ) ;
#7347 = ORIENTED_EDGE ( 'NONE', *, *, #2168, .F. ) ;
#7348 = ORIENTED_EDGE ( 'NONE', *, *, #14666, .T. ) ;
#7349 = MECHANICAL_DESIGN_GEOMETRIC_PRESENTATION_REPRESENTATION (  '', ( #13706 ), #14216 ) ;
#7350 = ORIENTED_EDGE ( 'NONE', *, *, #15855, .T. ) ;
#7351 = ADVANCED_FACE ( 'NONE', ( #440 ), #11377, .F. ) ;
#7352 = CARTESIAN_POINT ( 'NONE',  ( 30.02326902268086428, -5.673578940050561847, 7.939653947423658487 ) ) ;
#7353 = LINE ( 'NONE', #16963, #7922 ) ;
#7354 =( BOUNDED_CURVE ( )  B_SPLINE_CURVE ( 2, ( #14828, #9198, #16112, #3596, #12181 ),
 .UNSPECIFIED., .F., .T. ) 
 B_SPLINE_CURVE_WITH_KNOTS ( ( 3, 2, 3 ),
 ( 0.000000000000000000, 0.01282051282051282007, 0.01923076923076925265 ),
 .UNSPECIFIED. ) 
 CURVE ( )  GEOMETRIC_REPRESENTATION_ITEM ( )  RATIONAL_B_SPLINE_CURVE ( ( 1.000000000000000000, 0.8660254037844387076, 1.000000000000000000, 0.9330127018922191873, 0.9330127018922194093 ) ) 
 REPRESENTATION_ITEM ( '' )  );
#7355 = CARTESIAN_POINT ( 'NONE',  ( 15.92260893619738837, -28.39189527176317540, -12.00000000000000000 ) ) ;
#7356 = CARTESIAN_POINT ( 'NONE',  ( 0.000000000000000000, 3.000000000000000000, 2.399999999999999467 ) ) ;
#7357 = DIRECTION ( 'NONE',  ( 0.9937818688019538493, -0.1113444980252557837, 0.000000000000000000 ) ) ;
#7358 = CARTESIAN_POINT ( 'NONE',  ( 25.83772294520678159, -3.669972453104032084, -3.627061608673662896 ) ) ;
#7359 = CYLINDRICAL_SURFACE ( 'NONE', #4948, 2.499999999999999112 ) ;
#7360 = DIRECTION ( 'NONE',  ( 0.000000000000000000, 0.000000000000000000, -1.000000000000000000 ) ) ;
#7361 = CARTESIAN_POINT ( 'NONE',  ( 16.75000000000000000, -16.21813761408365195, 13.00000000000000178 ) ) ;
#7362 = CARTESIAN_POINT ( 'NONE',  ( 25.95846283556873502, -3.455553161483296609, -8.283357778048658915 ) ) ;
#7363 = VERTEX_POINT ( 'NONE', #10110 ) ;
#7364 = AXIS2_PLACEMENT_3D ( 'NONE', #10843, #12038, #13325 ) ;
#7365 = CARTESIAN_POINT ( 'NONE',  ( 33.44685390376565692, -4.007163506710925027, -7.939653947423662039 ) ) ;
#7366 = LINE ( 'NONE', #5887, #13345 ) ;
#7367 = DIRECTION ( 'NONE',  ( 0.000000000000000000, 0.000000000000000000, 1.000000000000000000 ) ) ;
#7368 = DIRECTION ( 'NONE',  ( 0.000000000000000000, 0.000000000000000000, -1.000000000000000000 ) ) ;
#7369 = DIRECTION ( 'NONE',  ( -0.1196152422706599633, 0.9928203230275514102, 0.000000000000000000 ) ) ;
#7370 = CARTESIAN_POINT ( 'NONE',  ( 29.27960797773944179, -6.689954721521948144, 7.033357778048657138 ) ) ;
#7371 = CARTESIAN_POINT ( 'NONE',  ( 26.88845778707760914, -3.543379655034240905, -7.939653947423660263 ) ) ;
#7372 = VERTEX_POINT ( 'NONE', #3241 ) ;
#7373 = ADVANCED_FACE ( 'NONE', ( #612 ), #1893, .T. ) ;
#7374 = ADVANCED_FACE ( 'NONE', ( #9930 ), #10209, .T. ) ;
#7375 = DIRECTION ( 'NONE',  ( 0.000000000000000000, 0.000000000000000000, 1.000000000000000000 ) ) ;
#7376 = ORIENTED_EDGE ( 'NONE', *, *, #3168, .T. ) ;
#7377 = VERTEX_POINT ( 'NONE', #8496 ) ;
#7378 = CARTESIAN_POINT ( 'NONE',  ( -45.00000000000000711, 0.000000000000000000, -5.537981825772250843 ) ) ;
#7379 = ORIENTED_EDGE ( 'NONE', *, *, #12885, .T. ) ;
#7380 = CARTESIAN_POINT ( 'NONE',  ( 27.14244485254070938, -4.766720295129625029, -7.939653947423662039 ) ) ;
#7381 = CARTESIAN_POINT ( 'NONE',  ( 25.93489015466116854, -5.606035894254070229, -7.939653947423662927 ) ) ;
#7382 = B_SPLINE_CURVE_WITH_KNOTS ( 'NONE', 3,
 ( #12943, #450, #14405, #10029, #13035, #16764, #8508, #7247, #11390, #9847, #12763, #10121, #7512, #15491, #15766, #4691, #1986, #16865 ),
 .UNSPECIFIED., .F., .F.,
 ( 4, 2, 2, 2, 2, 2, 2, 2, 4 ),
 ( 0.000000000000000000, 0.0005705796246920901435, 0.001141159249384180287, 0.001711738874076270539, 0.002282318498768360574, 0.002852898123460450609, 0.003423477748152541078, 0.003994057372844630679, 0.004564636997536721148 ),
 .UNSPECIFIED. ) ;
#7383 = CARTESIAN_POINT ( 'NONE',  ( 30.65370992780335868, -5.597623261208691581, -3.627061608673667781 ) ) ;
#7384 = ORIENTED_EDGE ( 'NONE', *, *, #562, .F. ) ;
#7385 = CARTESIAN_POINT ( 'NONE',  ( -2.540000000000001368, 3.110602869834278640E-16, 1.599999999999998979 ) ) ;
#7386 = CARTESIAN_POINT ( 'NONE',  ( -10.50000000000000000, 0.000000000000000000, -7.794427190999915211 ) ) ;
#7387 = LINE ( 'NONE', #9981, #11186 ) ;
#7388 = CARTESIAN_POINT ( 'NONE',  ( 31.12210306526553083, -4.287250072544045665, -8.283357778048662468 ) ) ;
#7389 = CARTESIAN_POINT ( 'NONE',  ( 0.000000000000000000, 0.000000000000000000, -2.000000000000000000 ) ) ;
#7390 = CARTESIAN_POINT ( 'NONE',  ( 32.54050588463559990, -2.235448945602741766, 4.705209693361167567 ) ) ;
#7391 = VERTEX_POINT ( 'NONE', #14030 ) ;
#7392 = EDGE_CURVE ( 'NONE', #2839, #13145, #9825, .T. ) ;
#7393 = CARTESIAN_POINT ( 'NONE',  ( 0.000000000000000000, 0.000000000000000000, -2.000000000000000000 ) ) ;
#7394 = LINE ( 'NONE', #129, #9833 ) ;
#7395 = LINE ( 'NONE', #12818, #17379 ) ;
#7396 = ORIENTED_EDGE ( 'NONE', *, *, #12273, .F. ) ;
#7397 = CARTESIAN_POINT ( 'NONE',  ( 31.05948030073166066, -1.776715885202022394, 5.783357778048665132 ) ) ;
#7398 = ORIENTED_EDGE ( 'NONE', *, *, #5453, .F. ) ;
#7399 = FACE_OUTER_BOUND ( 'NONE', #15267, .T. ) ;
#7400 = DIRECTION ( 'NONE',  ( 1.000000000000000000, 0.000000000000000000, 0.000000000000000000 ) ) ;
#7401 = VERTEX_POINT ( 'NONE', #2166 ) ;
#7402 = ORIENTED_EDGE ( 'NONE', *, *, #8369, .F. ) ;
#7403 = CARTESIAN_POINT ( 'NONE',  ( 34.51156627690993162, -8.531090163810741700, -5.783357778048662468 ) ) ;
#7404 = EDGE_CURVE ( 'NONE', #15290, #11575, #2423, .T. ) ;
#7405 = CARTESIAN_POINT ( 'NONE',  ( 31.67744797322171735, -2.039621600994187656, -7.033357778048658027 ) ) ;
#7406 = FACE_OUTER_BOUND ( 'NONE', #624, .T. ) ;
#7407 = CARTESIAN_POINT ( 'NONE',  ( 4.281152949374537720, 4.203775615332211224, -2.000000000000000000 ) ) ;
#7408 = CARTESIAN_POINT ( 'NONE',  ( 32.91278983782564183, -5.325448745358647429, -7.939653947423664704 ) ) ;
#7409 = DIRECTION ( 'NONE',  ( -0.000000000000000000, -0.000000000000000000, -1.000000000000000000 ) ) ;
#7410 = CARTESIAN_POINT ( 'NONE',  ( 30.92509028327567933, -4.310986222078405206, 3.627061608673664228 ) ) ;
#7411 = ORIENTED_EDGE ( 'NONE', *, *, #6271, .T. ) ;
#7412 = DIRECTION ( 'NONE',  ( 0.9928203230275510771, 0.1196152422706610596, 9.614813431917826478E-17 ) ) ;
#7413 = EDGE_CURVE ( 'NONE', #2945, #14967, #10637, .T. ) ;
#7414 = EDGE_LOOP ( 'NONE', ( #14521, #9054, #11237, #2041 ) ) ;
#7415 = CARTESIAN_POINT ( 'NONE',  ( 26.36761712467744090, -6.740983333149474177, 6.861505862736158257 ) ) ;
#7416 = CARTESIAN_POINT ( 'NONE',  ( -50.00000000000000000, -19.03270077640483038, 5.537981825772250843 ) ) ;
#7417 = CARTESIAN_POINT ( 'NONE',  ( 26.01595305975170547, -2.384361315936983416, -5.783357778048670461 ) ) ;
#7418 = ORIENTED_EDGE ( 'NONE', *, *, #510, .T. ) ;
#7419 = CARTESIAN_POINT ( 'NONE',  ( 45.00000000000000711, -16.03270077640482683, 10.53798182577225084 ) ) ;
#7420 = CARTESIAN_POINT ( 'NONE',  ( -4.000000000000000000, 0.8576023918602336815, -3.133238574225035933 ) ) ;
#7421 = CARTESIAN_POINT ( 'NONE',  ( -8.776279441628744848, 6.799038105676760146, -3.000000000000000888 ) ) ;
#7422 = EDGE_CURVE ( 'NONE', #10468, #8221, #2043, .T. ) ;
#7423 = CARTESIAN_POINT ( 'NONE',  ( 27.50829672905005907, -3.268828784122927100, -3.283357778048662023 ) ) ;
#7424 = DIRECTION ( 'NONE',  ( -1.000000000000000000, 0.000000000000000000, 0.000000000000000000 ) ) ;
#7425 = DIRECTION ( 'NONE',  ( 0.9928203230275510771, 0.1196152422706609902, 4.006172263299092517E-17 ) ) ;
#7426 = CARTESIAN_POINT ( 'NONE',  ( 26.98483462626008134, -4.785709214840094816, -7.939653947423662039 ) ) ;
#7427 = CARTESIAN_POINT ( 'NONE',  ( 28.13873763417255347, -3.192873105281056390, 8.283357778048666020 ) ) ;
#7428 = CARTESIAN_POINT ( 'NONE',  ( 31.67744797322171735, -2.039621600994187656, 4.533357778048667797 ) ) ;
#7429 = EDGE_LOOP ( 'NONE', ( #11610, #11507, #8209, #9876, #9648, #1385 ) ) ;
#7430 = ADVANCED_FACE ( 'NONE', ( #4852 ), #2072, .F. ) ;
#7431 = ORIENTED_EDGE ( 'NONE', *, *, #8634, .T. ) ;
#7432 = DIRECTION ( 'NONE',  ( -0.8660254037844397068, -0.4999999999999981126, 0.000000000000000000 ) ) ;
#7433 = CARTESIAN_POINT ( 'NONE',  ( 31.54230778485832332, -2.355712103769039611, 6.861505862736166250 ) ) ;
#7434 = FACE_OUTER_BOUND ( 'NONE', #17162, .T. ) ;
#7435 = CARTESIAN_POINT ( 'NONE',  ( 20.00000000000000000, 7.999999999999996447, -12.00000000000000000 ) ) ;
#7436 = CARTESIAN_POINT ( 'NONE',  ( 10.50000000000000000, 1.285879139104720831E-15, -6.005572809000082835 ) ) ;
#7437 = CARTESIAN_POINT ( 'NONE',  ( 32.30426898124760982, -6.025734024055190652, -6.861505862736167138 ) ) ;
#7438 = CARTESIAN_POINT ( 'NONE',  ( -37.55714628004649569, -12.56174331051002113, -5.783357778048663356 ) ) ;
#7439 = CARTESIAN_POINT ( 'NONE',  ( 27.41826274939272423, -4.733489685532582314, -8.283357778048662468 ) ) ;
#7440 = CARTESIAN_POINT ( 'NONE',  ( -4.211140560182196957, 2.431303136016540911, -3.445885042887435468 ) ) ;
#7441 = CARTESIAN_POINT ( 'NONE',  ( 27.73348320195396965, -4.695511846111656062, -3.283357778048664688 ) ) ;
#7442 = CYLINDRICAL_SURFACE ( 'NONE', #11070, 2.500000000000001776 ) ;
#7443 = ORIENTED_EDGE ( 'NONE', *, *, #9142, .T. ) ;
#7444 = EDGE_CURVE ( 'NONE', #4560, #14120, #9439, .T. ) ;
#7445 = CARTESIAN_POINT ( 'NONE',  ( 26.36761712467744090, -6.740983333149474177, -4.705209693361168455 ) ) ;
#7446 = DIRECTION ( 'NONE',  ( 1.000000000000000000, 0.000000000000000000, 0.000000000000000000 ) ) ;
#7447 = CARTESIAN_POINT ( 'NONE',  ( 32.77701044293393551, -4.087866415376695706, -3.283357778048664688 ) ) ;
#7448 = CARTESIAN_POINT ( 'NONE',  ( 4.197393957002304887, 7.725818140447171444E-14, -3.203767560748932208 ) ) ;
#7449 = FACE_OUTER_BOUND ( 'NONE', #14319, .T. ) ;
#7450 = CARTESIAN_POINT ( 'NONE',  ( 28.51030546511822195, -6.055733689321201041, 8.283357778048658915 ) ) ;
#7451 = ORIENTED_EDGE ( 'NONE', *, *, #11508, .F. ) ;
#7452 = CARTESIAN_POINT ( 'NONE',  ( 30.88577694472199298, -6.196634301449400084, -6.861505862736166250 ) ) ;
#7453 = ORIENTED_EDGE ( 'NONE', *, *, #8915, .F. ) ;
#7454 = CARTESIAN_POINT ( 'NONE',  ( 10.47816170930907553, -0.6768509389586216951, -7.794427190999915211 ) ) ;
#7455 = CARTESIAN_POINT ( 'NONE',  ( 35.77680296528374271, -19.03270077640483038, -0.5379818257722512875 ) ) ;
#7456 = ORIENTED_EDGE ( 'NONE', *, *, #17205, .F. ) ;
#7457 = CARTESIAN_POINT ( 'NONE',  ( 26.41562710823574278, -3.600346414165641828, -7.939653947423660263 ) ) ;
#7458 = CARTESIAN_POINT ( 'NONE',  ( -10.50000000000000000, 0.000000000000000000, -10.00000000000000000 ) ) ;
#7459 = AXIS2_PLACEMENT_3D ( 'NONE', #7389, #12903, #12159 ) ;
#7460 = ADVANCED_FACE ( 'NONE', ( #7596 ), #13120, .F. ) ;
#7461 = CARTESIAN_POINT ( 'NONE',  ( 28.23249303296521617, -2.754479417688857179, -4.705209693361161349 ) ) ;
#7462 = VERTEX_POINT ( 'NONE', #13390 ) ;
#7463 = DIRECTION ( 'NONE',  ( 5.026720092345836698E-22, -4.581671729415424240E-22, 1.000000000000000000 ) ) ;
#7464 = FACE_OUTER_BOUND ( 'NONE', #16664, .T. ) ;
#7465 = CARTESIAN_POINT ( 'NONE',  ( 27.21934464581372737, -3.303641803799556964, -8.283357778048658915 ) ) ;
#7466 = LINE ( 'NONE', #14171, #7171 ) ;
#7467 = VERTEX_POINT ( 'NONE', #6313 ) ;
#7468 = CARTESIAN_POINT ( 'NONE',  ( 32.65880277236253448, -4.102108105263264193, 3.627061608673664228 ) ) ;
#7469 = AXIS2_PLACEMENT_3D ( 'NONE', #12632, #220, #5730 ) ;
#7470 = ORIENTED_EDGE ( 'NONE', *, *, #11698, .F. ) ;
#7471 = DIRECTION ( 'NONE',  ( -5.026720092345836698E-22, 4.581671729415424240E-22, -1.000000000000000000 ) ) ;
#7472 = DIRECTION ( 'NONE',  ( -0.9937818688019538493, -0.1113444980252557837, 0.000000000000000000 ) ) ;
#7473 = FACE_BOUND ( 'NONE', #15221, .T. ) ;
#7474 = ORIENTED_EDGE ( 'NONE', *, *, #9395, .T. ) ;
#7475 = CARTESIAN_POINT ( 'NONE',  ( 28.11132641904908169, -7.168068194032743534, -5.783357778048668685 ) ) ;
#7476 = ORIENTED_EDGE ( 'NONE', *, *, #1846, .T. ) ;
#7477 = CARTESIAN_POINT ( 'NONE',  ( 3.443595183066687326, -15.28297513750540837, -16.99984776326510172 ) ) ;
#7478 = CARTESIAN_POINT ( 'NONE',  ( 26.61898274975073164, -6.283600725846810953, -3.283357778048667797 ) ) ;
#7479 = CARTESIAN_POINT ( 'NONE',  ( 30.63309003953906995, -6.864245478665264244, -5.783357778048663356 ) ) ;
#7480 = CARTESIAN_POINT ( 'NONE',  ( 28.16881664323205570, -6.096876348486420127, -8.283357778048662468 ) ) ;
#7481 = CYLINDRICAL_SURFACE ( 'NONE', #15366, 5.000000000000001776 ) ;
#7482 = EDGE_CURVE ( 'NONE', #60, #602, #11927, .T. ) ;
#7483 = CONTEXT_DEPENDENT_SHAPE_REPRESENTATION ( #330, #13156 ) ;
#7484 = CARTESIAN_POINT ( 'NONE',  ( -6.000000000000000888, 0.000000000000000000, -2.000000000000000000 ) ) ;
#7485 = CARTESIAN_POINT ( 'NONE',  ( 32.50119254608192421, -4.121097024973739309, -3.627061608673664672 ) ) ;
#7486 = VECTOR ( 'NONE', #2804, 999.9999999999998863 ) ;
#7487 = CARTESIAN_POINT ( 'NONE',  ( 26.31556265977298992, -7.384422263489805793, 5.783357778048663356 ) ) ;
#7489 = DIRECTION ( 'NONE',  ( 0.000000000000000000, 0.000000000000000000, -1.000000000000000000 ) ) ;
#7488 = CIRCLE ( 'NONE', #4872, 3.999999999999994671 ) ;
#7490 = CARTESIAN_POINT ( 'NONE',  ( 26.60838078660069428, -6.085005533777348319, 3.627061608673662896 ) ) ;
#7491 = ORIENTED_EDGE ( 'NONE', *, *, #603, .F. ) ;
#7492 = CIRCLE ( 'NONE', #14152, 5.384454397937117776 ) ;
#7493 = CARTESIAN_POINT ( 'NONE',  ( 26.31308423962587995, -7.363851090081250383, 5.766985353495324595 ) ) ;
#7494 = VERTEX_POINT ( 'NONE', #11834 ) ;
#7495 = CARTESIAN_POINT ( 'NONE',  ( 32.06767520579373354, -2.292415704734142690, 4.705209693361168455 ) ) ;
#7496 = CARTESIAN_POINT ( 'NONE',  ( -24.42951923951777005, -10.13045284482685382, 14.60898600760630472 ) ) ;
#7497 = CARTESIAN_POINT ( 'NONE',  ( 27.19802975513453092, -2.241944418315925613, -5.783357778048658027 ) ) ;
#7498 = ORIENTED_EDGE ( 'NONE', *, *, #1481, .T. ) ;
#7499 = CYLINDRICAL_SURFACE ( 'NONE', #10788, 2.749999999999992895 ) ;
#7500 = VECTOR ( 'NONE', #12126, 1000.000000000000000 ) ;
#7501 = CARTESIAN_POINT ( 'NONE',  ( -4.197312189423712425, -0.8182410726374559351, -3.202520316362482244 ) ) ;
#7502 = VERTEX_POINT ( 'NONE', #17412 ) ;
#7503 = DIRECTION ( 'NONE',  ( -0.8660254037844329345, 0.5000000000000099920, 0.000000000000000000 ) ) ;
#7504 = PLANE ( 'NONE',  #16605 ) ;
#7505 = CARTESIAN_POINT ( 'NONE',  ( 25.63782166807609997, -6.407846580969937200, -7.820349034508990549 ) ) ;
#7506 = CARTESIAN_POINT ( 'NONE',  ( 27.11643206945770146, -20.93856092459426677, 13.95341982493238753 ) ) ;
#7507 = LINE ( 'NONE', #6140, #1148 ) ;
#7508 = CARTESIAN_POINT ( 'NONE',  ( 26.46816385032927599, -3.594016774262162706, -3.627061608673662896 ) ) ;
#7509 = ORIENTED_EDGE ( 'NONE', *, *, #10513, .F. ) ;
#7510 = VECTOR ( 'NONE', #16679, 1000.000000000000227 ) ;
#7511 = ADVANCED_FACE ( 'NONE', ( #6499 ), #15841, .T. ) ;
#7512 = CARTESIAN_POINT ( 'NONE',  ( 25.83183225892938140, -3.369404079293177645, -7.443282702368841264 ) ) ;
#7513 = CARTESIAN_POINT ( 'NONE',  ( 32.61569110240115776, -6.288022587442930522, 4.533357778048659803 ) ) ;
#7514 = AXIS2_PLACEMENT_3D ( 'NONE', #353, #618, #11188 ) ;
#7515 = EDGE_LOOP ( 'NONE', ( #1594, #135, #2047, #3582 ) ) ;
#7516 = ADVANCED_FACE ( 'NONE', ( #1055 ), #12014, .T. ) ;
#7517 = EDGE_CURVE ( 'NONE', #16901, #13349, #17597, .T. ) ;
#7518 = ORIENTED_EDGE ( 'NONE', *, *, #14055, .F. ) ;
#7519 = ORIENTED_EDGE ( 'NONE', *, *, #13177, .T. ) ;
#7520 = DIRECTION ( 'NONE',  ( 0.000000000000000000, 0.000000000000000000, 1.000000000000000000 ) ) ;
#7521 = VECTOR ( 'NONE', #15847, 1000.000000000000227 ) ;
#7522 = CARTESIAN_POINT ( 'NONE',  ( 32.70264286945147347, -5.350767304972614546, 7.939653947423658487 ) ) ;
#7523 = DIRECTION ( 'NONE',  ( -0.000000000000000000, -1.000000000000000000, -0.000000000000000000 ) ) ;
#7524 = CARTESIAN_POINT ( 'NONE',  ( -14.05523583925745257, 13.74128089903392613, -16.39434919531312218 ) ) ;
#7525 = CARTESIAN_POINT ( 'NONE',  ( -29.25000000000000000, -16.63595338719256844, -13.37255996287877124 ) ) ;
#7526 = CARTESIAN_POINT ( 'NONE',  ( 26.24062359194589078, -6.129313013101781671, -3.627061608673667781 ) ) ;
#7527 = DIRECTION ( 'NONE',  ( 0.000000000000000000, 0.000000000000000000, -1.000000000000000000 ) ) ;
#7528 = DIRECTION ( 'NONE',  ( -0.9928203230275512992, -0.1196152422706610180, -9.614813431917824012E-17 ) ) ;
#7529 = AXIS2_PLACEMENT_3D ( 'NONE', #719, #15960, #11764 ) ;
#7530 = CARTESIAN_POINT ( 'NONE',  ( -0.6937372685066658384, 4.453844082567720797, -3.310536846335889738 ) ) ;
#7531 = CARTESIAN_POINT ( 'NONE',  ( 38.94468999590795733, -1.453587954722214137, -2.531230242176644829 ) ) ;
#7532 = CARTESIAN_POINT ( 'NONE',  ( 28.13948077428293715, -7.164676150231702678, -6.453230759126474148 ) ) ;
#7533 = ORIENTED_EDGE ( 'NONE', *, *, #15138, .F. ) ;
#7534 = ORIENTED_EDGE ( 'NONE', *, *, #16958, .T. ) ;
#7535 = ADVANCED_FACE ( 'NONE', ( #874 ), #17514, .F. ) ;
#7536 = CARTESIAN_POINT ( 'NONE',  ( 27.08121146544255353, -6.028038774645947839, -7.939653947423664704 ) ) ;
#7537 = DIRECTION ( 'NONE',  ( -0.1196152422706610735, 0.9928203230275511881, 0.000000000000000000 ) ) ;
#7538 = DIRECTION ( 'NONE',  ( 0.9899494936611662466, -0.1414213562373111965, 0.000000000000000000 ) ) ;
#7539 = CARTESIAN_POINT ( 'NONE',  ( 27.18555652250208610, -2.580805812949960920, 4.533357778048667797 ) ) ;
#7540 = EDGE_CURVE ( 'NONE', #13908, #15040, #6392, .T. ) ;
#7541 = VECTOR ( 'NONE', #13295, 1000.000000000000000 ) ;
#7542 = ORIENTED_EDGE ( 'NONE', *, *, #2762, .F. ) ;
#7543 = CARTESIAN_POINT ( 'NONE',  ( -16.75000000000000000, -16.21813761408365195, -13.00000000000000178 ) ) ;
#7544 = CARTESIAN_POINT ( 'NONE',  ( 30.90769699326645181, -6.820963901304073929, -5.783357778048668685 ) ) ;
#7545 = ORIENTED_EDGE ( 'NONE', *, *, #8798, .F. ) ;
#7546 = EDGE_CURVE ( 'NONE', #2213, #4427, #9207, .T. ) ;
#7547 = DIRECTION ( 'NONE',  ( 0.000000000000000000, 0.000000000000000000, -1.000000000000000000 ) ) ;
#7548 = VECTOR ( 'NONE', #5551, 1000.000000000000114 ) ;
#7549 = CARTESIAN_POINT ( 'NONE',  ( 31.26353094466156080, -6.788289799823394866, -5.783357778048663356 ) ) ;
#7550 = ORIENTED_EDGE ( 'NONE', *, *, #11369, .F. ) ;
#7551 = CARTESIAN_POINT ( 'NONE',  ( 29.86122125502053848, -4.439161430227785310, -8.283357778048662468 ) ) ;
#7552 = CARTESIAN_POINT ( 'NONE',  ( 27.10313151398701947, -6.652368374500619908, -6.861505862736166250 ) ) ;
#7553 = CARTESIAN_POINT ( 'NONE',  ( -2.000000000000002220, 3.464101615137751278, 0.000000000000000000 ) ) ;
#7554 = CARTESIAN_POINT ( 'NONE',  ( 33.78529456515154550, -6.484467084455914687, -5.783357778048663356 ) ) ;
#7555 = PLANE ( 'NONE',  #16170 ) ;
#7556 = ORIENTED_EDGE ( 'NONE', *, *, #11018, .T. ) ;
#7557 = CARTESIAN_POINT ( 'NONE',  ( 28.69037342443288452, -3.126411886501869741, -3.283357778048662023 ) ) ;
#7558 = CARTESIAN_POINT ( 'NONE',  ( 27.17934203385504333, -30.00000000000000355, 13.93658524716016878 ) ) ;
#7559 = AXIS2_PLACEMENT_3D ( 'NONE', #3019, #8541, #7192 ) ;
#7560 = CARTESIAN_POINT ( 'NONE',  ( 30.88125018618674744, -3.062327022369072171, 7.939653947423664704 ) ) ;
#7561 = AXIS2_PLACEMENT_3D ( 'NONE', #8893, #2011, #11691 ) ;
#7562 = VECTOR ( 'NONE', #5965, 1000.000000000000000 ) ;
#7563 = EDGE_CURVE ( 'NONE', #548, #15612, #16210, .T. ) ;
#7564 = ORIENTED_EDGE ( 'NONE', *, *, #14893, .F. ) ;
#7565 = CARTESIAN_POINT ( 'NONE',  ( 30.57046727500519978, -4.353711291323232757, -8.283357778048662468 ) ) ;
#7566 = LINE ( 'NONE', #3388, #12746 ) ;
#7567 = CARTESIAN_POINT ( 'NONE',  ( -1.500000000000000000, -11.00000000000000000, -3.000000000000000000 ) ) ;
#7568 = ORIENTED_EDGE ( 'NONE', *, *, #4788, .F. ) ;
#7569 = CARTESIAN_POINT ( 'NONE',  ( -10.37836969302994028, 0.6704047395399693743, -6.899999999999998579 ) ) ;
#7570 = CARTESIAN_POINT ( 'NONE',  ( 25.87953856062030766, -3.765371892057810754, -3.950981403410641857 ) ) ;
#7571 = DIRECTION ( 'NONE',  ( 0.9928203230275512992, 0.1196152422706614898, -0.000000000000000000 ) ) ;
#7572 = CARTESIAN_POINT ( 'NONE',  ( -1.500000000000000000, 11.00000000000000000, -2.000000000000000000 ) ) ;
#7573 = AXIS2_PLACEMENT_3D ( 'NONE', #399, #661, #10167 ) ;
#7574 = ADVANCED_FACE ( 'NONE', ( #4032 ), #12158, .T. ) ;
#7575 = CARTESIAN_POINT ( 'NONE',  ( 28.52524344760924180, -2.419399995203538101, -7.033357778048658027 ) ) ;
#7576 = FACE_BOUND ( 'NONE', #6092, .T. ) ;
#7577 = DIRECTION ( 'NONE',  ( 0.9928203230275510771, 0.1196152422706609902, 4.006172263299092517E-17 ) ) ;
#7578 = ORIENTED_EDGE ( 'NONE', *, *, #8159, .F. ) ;
#7579 = CARTESIAN_POINT ( 'NONE',  ( 31.55553118839817728, -4.235030543236534939, -7.939653947423662039 ) ) ;
#7580 = VECTOR ( 'NONE', #6107, 1000.000000000000000 ) ;
#7581 = CARTESIAN_POINT ( 'NONE',  ( -13.00000000000000178, 1.592040838891559293E-15, -8.700000000000001066 ) ) ;
#7582 = DIRECTION ( 'NONE',  ( 0.000000000000000000, 0.000000000000000000, -1.000000000000000000 ) ) ;
#7583 = CARTESIAN_POINT ( 'NONE',  ( 27.78610916120306129, -6.570083055755264745, 6.861505862736157368 ) ) ;
#7584 = B_SPLINE_CURVE_WITH_KNOTS ( 'NONE', 3,
 ( #2027, #16412, #78, #11105, #1436, #13593, #7068, #13680, #4165, #12584, #12228, #9409, #8408, #17883, #2621, #9493, #15126, #15034, #10845, #3893, #12491, #13940, #3979, #1175, #9747, #13848, #17965, #8318, #8148, #6960, #2881, #12317, #1533, #4247, #1269, #163, #15300, #10925, #14950, #6787, #17802, #5322, #5675, #5409 ),
 .UNSPECIFIED., .F., .F.,
 ( 4, 2, 2, 2, 2, 2, 2, 2, 2, 2, 2, 2, 2, 2, 2, 2, 2, 2, 2, 2, 2, 4 ),
 ( 0.000000000000000000, 0.001235617314710323825, 0.001853425972065488340, 0.002471234629420653289, 0.003706851944130986655, 0.004324660601486156157, 0.004942469258841326527, 0.006178086573551669868, 0.007413703888262013209, 0.008031512545617180976, 0.008649321202972348743, 0.009884938517682682543, 0.01112055583239301808, 0.01235617314710335361, 0.01297398180445852138, 0.01359179046181369088, 0.01482740777652402121, 0.01606302509123435501, 0.01668083374858951584, 0.01729864240594468014, 0.01853425972065500180, 0.01976987703536532692 ),
 .UNSPECIFIED. ) ;
#7585 = AXIS2_PLACEMENT_3D ( 'NONE', #11276, #8311, #11182 ) ;
#7586 = ORIENTED_EDGE ( 'NONE', *, *, #756, .F. ) ;
#7587 = CARTESIAN_POINT ( 'NONE',  ( 26.21417678486618641, -2.370676134166772808, -5.783357778048658027 ) ) ;
#7588 = VERTEX_POINT ( 'NONE', #6839 ) ;
#7589 = EDGE_CURVE ( 'NONE', #6677, #1421, #11863, .T. ) ;
#7590 = CARTESIAN_POINT ( 'NONE',  ( 32.19919549706052209, -6.038393303862174655, 6.861505862736157368 ) ) ;
#7591 = DIRECTION ( 'NONE',  ( 0.000000000000000000, 0.000000000000000000, 1.000000000000000000 ) ) ;
#7592 = LINE ( 'NONE', #16207, #3562 ) ;
#7593 = ORIENTED_EDGE ( 'NONE', *, *, #12167, .T. ) ;
#7594 = AXIS2_PLACEMENT_3D ( 'NONE', #6825, #12271, #17919 ) ;
#7595 = AXIS2_PLACEMENT_3D ( 'NONE', #14161, #478, #7284 ) ;
#7596 = FACE_OUTER_BOUND ( 'NONE', #12303, .T. ) ;
#7597 = LINE ( 'NONE', #972, #17755 ) ;
#7598 = CARTESIAN_POINT ( 'NONE',  ( -5.781152949374509298, 1.605699403978973372, -2.000000000000000000 ) ) ;
#7599 = CARTESIAN_POINT ( 'NONE',  ( 27.60595198473284384, -7.618504009027492252, -5.783357778048669573 ) ) ;
#7600 = DIRECTION ( 'NONE',  ( 0.000000000000000000, 0.000000000000000000, 1.000000000000000000 ) ) ;
#7601 = AXIS2_PLACEMENT_3D ( 'NONE', #8678, #4676, #15561 ) ;
#7602 = CARTESIAN_POINT ( 'NONE',  ( 26.01652455409633902, -4.902371455920928156, -5.783357778048663356 ) ) ;
#7603 = CARTESIAN_POINT ( 'NONE',  ( 26.25801688195511474, -3.619335333876111171, -7.939653947423660263 ) ) ;
#7604 = CARTESIAN_POINT ( 'NONE',  ( 0.000000000000000000, 0.000000000000000000, -2.000000000000000000 ) ) ;
#7605 = CIRCLE ( 'NONE', #10488, 5.500000000000000888 ) ;
#7606 = CARTESIAN_POINT ( 'NONE',  ( 32.51061761821408425, -6.300681867249914525, 7.033357778048657138 ) ) ;
#7607 = CIRCLE ( 'NONE', #7891, 0.9000000000000011324 ) ;
#7608 = VERTEX_POINT ( 'NONE', #9548 ) ;
#7609 = ORIENTED_EDGE ( 'NONE', *, *, #11922, .F. ) ;
#7610 =( BOUNDED_CURVE ( )  B_SPLINE_CURVE ( 2, ( #3151, #16859, #6039, #1711, #16952 ),
 .UNSPECIFIED., .F., .T. ) 
 B_SPLINE_CURVE_WITH_KNOTS ( ( 3, 2, 3 ),
 ( 0.000000000000000000, 0.01282051282051282007, 0.01923076923076924571 ),
 .UNSPECIFIED. ) 
 CURVE ( )  GEOMETRIC_REPRESENTATION_ITEM ( )  RATIONAL_B_SPLINE_CURVE ( ( 1.000000000000000000, 0.8660254037844387076, 1.000000000000000000, 0.9330127018922191873, 0.9330127018922194093 ) ) 
 REPRESENTATION_ITEM ( '' )  );
#7611 = ORIENTED_EDGE ( 'NONE', *, *, #17011, .T. ) ;
#7612 = CARTESIAN_POINT ( 'NONE',  ( 27.48088551392658729, -7.244023872874614689, 5.783357778048669573 ) ) ;
#7613 = AXIS2_PLACEMENT_3D ( 'NONE', #11373, #14026, #11558 ) ;
#7614 =( REPRESENTATION_RELATIONSHIP ('NONE','NONE', #3227, #16332 ) REPRESENTATION_RELATIONSHIP_WITH_TRANSFORMATION ( #10001 )SHAPE_REPRESENTATION_RELATIONSHIP( ) );
#7615 = LINE ( 'NONE', #12951, #1264 ) ;
#7616 = CARTESIAN_POINT ( 'NONE',  ( 4.281152949374507521, -4.203775615332241422, -1.901951201008075243 ) ) ;
#7617 = EDGE_CURVE ( 'NONE', #15284, #11466, #12236, .T. ) ;
#7618 = CARTESIAN_POINT ( 'NONE',  ( -19.90989778724008019, -21.66613080872904717, -15.52824432210780259 ) ) ;
#7619 = CARTESIAN_POINT ( 'NONE',  ( 32.93018312783485158, -2.815471066132994249, -3.627061608673662008 ) ) ;
#7620 = CARTESIAN_POINT ( 'NONE',  ( 30.64556327217151122, -6.525384084031224496, -7.033357778048666908 ) ) ;
#7621 = CARTESIAN_POINT ( 'NONE',  ( 25.11802603177690330, -19.03270077640483038, -0.5379818257722508434 ) ) ;
#7622 = AXIS2_PLACEMENT_3D ( 'NONE', #16387, #4218, #12369 ) ;
#7623 = CARTESIAN_POINT ( 'NONE',  ( 17.88061427385022739, 10.54987872837076601, 15.87467694953868502 ) ) ;
#7624 = CARTESIAN_POINT ( 'NONE',  ( 20.27684169284606241, -10.57794632788464995, 15.46227570229628689 ) ) ;
#7625 = ADVANCED_FACE ( 'NONE', ( #8287 ), #13817, .F. ) ;
#7626 = SURFACE_STYLE_FILL_AREA ( #2280 ) ;
#7627 = ORIENTED_EDGE ( 'NONE', *, *, #11811, .F. ) ;
#7628 = ORIENTED_EDGE ( 'NONE', *, *, #137, .T. ) ;
#7629 = CARTESIAN_POINT ( 'NONE',  ( 27.72904566057427189, -3.442105416578422172, -3.627061608673662896 ) ) ;
#7630 = VECTOR ( 'NONE', #16949, 1000.000000000000227 ) ;
#7631 = CARTESIAN_POINT ( 'NONE',  ( 32.81641299864316608, -4.083119185552795294, -7.939653947423662039 ) ) ;
#7632 = ORIENTED_EDGE ( 'NONE', *, *, #3776, .T. ) ;
#7633 = CARTESIAN_POINT ( 'NONE',  ( 3.999999999999998224, -2.309401076758513582, -0.5000000000000000000 ) ) ;
#7634 = CARTESIAN_POINT ( 'NONE',  ( 27.24942365487322959, -6.207645047004941574, 8.283357778048658915 ) ) ;
#7635 = ORIENTED_EDGE ( 'NONE', *, *, #16853, .F. ) ;
#7636 = ORIENTED_EDGE ( 'NONE', *, *, #17816, .F. ) ;
#7637 = LINE ( 'NONE', #4802, #16445 ) ;
#7638 = CARTESIAN_POINT ( 'NONE',  ( 33.14902674121363901, -1.535163666906202318, -5.783357778048658915 ) ) ;
#7639 = ORIENTED_EDGE ( 'NONE', *, *, #1321, .F. ) ;
#7640 = EDGE_CURVE ( 'NONE', #7189, #317, #16464, .T. ) ;
#7641 = LINE ( 'NONE', #4807, #906 ) ;
#7642 = CARTESIAN_POINT ( 'NONE',  ( 25.83183225892938140, -3.369404079293177645, -7.443282702368841264 ) ) ;
#7643 = CARTESIAN_POINT ( 'NONE',  ( 33.60446413004628141, -3.988174587000466342, 7.939653947423662039 ) ) ;
#7644 = CARTESIAN_POINT ( 'NONE',  ( 3.455075492488604016, -2.624013387858240787, -3.016622336522134518 ) ) ;
#7645 = ORIENTED_EDGE ( 'NONE', *, *, #15322, .T. ) ;
#7646 = CARTESIAN_POINT ( 'NONE',  ( 27.15566825608056689, -6.646038734597135011, -4.705209693361169343 ) ) ;
#7647 = EDGE_CURVE ( 'NONE', #11700, #1184, #13033, .T. ) ;
#7648 = LINE ( 'NONE', #13171, #16766 ) ;
#7649 = CARTESIAN_POINT ( 'NONE',  ( -1.655952806101419927, 3.662737355149035423, -2.077348303141170793E-15 ) ) ;
#7650 = CARTESIAN_POINT ( 'NONE',  ( 27.45957062324739084, -6.182326487390971792, -8.283357778048664244 ) ) ;
#7651 = DIRECTION ( 'NONE',  ( -0.1196152422706584506, 0.9928203230275515212, 0.000000000000000000 ) ) ;
#7652 = CARTESIAN_POINT ( 'NONE',  ( 29.70732014299206369, -2.276983097582480742, -7.033357778048658027 ) ) ;
#7653 = LINE ( 'NONE', #14361, #2527 ) ;
#7654 = VERTEX_POINT ( 'NONE', #2588 ) ;
#7655 = CYLINDRICAL_SURFACE ( 'NONE', #6304, 2.500000000000000444 ) ;
#7656 = CARTESIAN_POINT ( 'NONE',  ( 2.344047193898586734, 3.265465875126468465, -1.231162388834125148E-15 ) ) ;
#7657 = CARTESIAN_POINT ( 'NONE',  ( 27.87986455999572399, -6.131689368163070419, 8.283357778048660691 ) ) ;
#7658 = ORIENTED_EDGE ( 'NONE', *, *, #14300, .T. ) ;
#7659 = PLANE ( 'NONE',  #6463 ) ;
#7660 = CARTESIAN_POINT ( 'NONE',  ( 31.07327543742414022, -2.112412460091767308, -4.533357778048659803 ) ) ;
#7661 = DIRECTION ( 'NONE',  ( 0.000000000000000000, -1.000000000000000000, 1.287488025362403787E-15 ) ) ;
#7662 = CARTESIAN_POINT ( 'NONE',  ( 33.58707084003705745, -6.498152266226124851, -5.783357778048669573 ) ) ;
#7663 = EDGE_LOOP ( 'NONE', ( #7201, #5778 ) ) ;
#7664 = ADVANCED_BREP_SHAPE_REPRESENTATION ( '', ( #17610, #3575 ), #12173 ) ;
#7665 = CARTESIAN_POINT ( 'NONE',  ( 29.94002636988270538, -4.429666970165102136, -8.283357778048662468 ) ) ;
#7666 = DIRECTION ( 'NONE',  ( -1.000000000000000000, 0.000000000000000000, 0.000000000000000000 ) ) ;
#7667 = CONTEXT_DEPENDENT_SHAPE_REPRESENTATION ( #10835, #4041 ) ;
#7668 = CARTESIAN_POINT ( 'NONE',  ( 26.01652455409633902, -4.902371455920926380, -5.783357778048663356 ) ) ;
#7669 = CARTESIAN_POINT ( 'NONE',  ( 26.01652455409633902, -4.902371455920928156, -5.783357778048663356 ) ) ;
#7670 = CARTESIAN_POINT ( 'NONE',  ( 29.52399153675929355, -1.971908820246954130, -5.783357778048658027 ) ) ;
#7671 = ADVANCED_FACE ( 'NONE', ( #6757 ), #8114, .F. ) ;
#7672 = CARTESIAN_POINT ( 'NONE',  ( 41.90164972253718645, -2.988527579590353422, -5.783357778048662468 ) ) ;
#7673 = DIRECTION ( 'NONE',  ( -0.6000000000000001998, -0.7999999999999999334, 0.000000000000000000 ) ) ;
#7674 = CARTESIAN_POINT ( 'NONE',  ( 28.54354359905709870, -7.105797696961086096, 5.783357778048657138 ) ) ;
#7675 = ORIENTED_EDGE ( 'NONE', *, *, #640, .F. ) ;
#7676 = CARTESIAN_POINT ( 'NONE',  ( 27.12505156253147476, -7.276697974355294640, -5.783357778048668685 ) ) ;
#7677 = ORIENTED_EDGE ( 'NONE', *, *, #15004, .F. ) ;
#7678 = CARTESIAN_POINT ( 'NONE',  ( 32.67619606237177265, -1.592130426037603907, 5.783357778048668685 ) ) ;
#7679 = CARTESIAN_POINT ( 'NONE',  ( -19.91444112663254984, -10.77903654349075246, 15.52697452096630748 ) ) ;
#7680 = CARTESIAN_POINT ( 'NONE',  ( 2.500000000000000888, 0.000000000000000000, -4.699999999999999289 ) ) ;
#7681 = EDGE_LOOP ( 'NONE', ( #7509, #2520 ) ) ;
#7682 = DIRECTION ( 'NONE',  ( -0.000000000000000000, -0.000000000000000000, 1.000000000000000000 ) ) ;
#7683 = CARTESIAN_POINT ( 'NONE',  ( 30.33776104811456165, -2.201027418740610919, 4.533357778048667797 ) ) ;
#7684 = CARTESIAN_POINT ( 'NONE',  ( 8.632250723006720250, -18.84644399697197770, -13.00000000000000178 ) ) ;
#7685 = CARTESIAN_POINT ( 'NONE',  ( 31.30154412293507349, -3.011689903141150815, -7.939653947423660263 ) ) ;
#7686 = DIRECTION ( 'NONE',  ( 0.000000000000000000, 0.000000000000000000, -1.000000000000000000 ) ) ;
#7687 = FACE_OUTER_BOUND ( 'NONE', #8303, .T. ) ;
#7688 =( NAMED_UNIT ( * ) SI_UNIT ( $, .STERADIAN. ) SOLID_ANGLE_UNIT ( ) );
#7689 = CARTESIAN_POINT ( 'NONE',  ( 27.12505156253147476, -7.276697974355294640, -5.783357778048668685 ) ) ;
#7690 = EDGE_CURVE ( 'NONE', #11059, #16386, #4344, .T. ) ;
#7691 = EDGE_CURVE ( 'NONE', #17723, #16561, #11988, .T. ) ;
#7692 = CARTESIAN_POINT ( 'NONE',  ( 25.96530230012339757, -2.390463732198628399, -5.113484796970851676 ) ) ;
#7693 = CARTESIAN_POINT ( 'NONE',  ( 30.75815651034531584, -7.238725614818142695, 5.783357778048657138 ) ) ;
#7694 = VERTEX_POINT ( 'NONE', #8376 ) ;
#7695 = EDGE_LOOP ( 'NONE', ( #5771, #16921 ) ) ;
#7696 = VERTEX_POINT ( 'NONE', #5203 ) ;
#7697 = CARTESIAN_POINT ( 'NONE',  ( 33.60446413004628141, -3.988174587000466342, 7.939653947423662039 ) ) ;
#7698 = CARTESIAN_POINT ( 'NONE',  ( 33.35047706458318828, -2.764833946905070672, 3.627061608673666449 ) ) ;
#7699 = SURFACE_STYLE_USAGE ( .BOTH. , #3527 ) ;
#7700 = CARTESIAN_POINT ( 'NONE',  ( 29.30958546476020743, -4.505622649006972402, -8.283357778048662468 ) ) ;
#7701 = CARTESIAN_POINT ( 'NONE',  ( -29.25000000000000000, -16.21813761408365195, -13.37255996287876947 ) ) ;
#7702 = CARTESIAN_POINT ( 'NONE',  ( 28.51709679197739078, -3.347160818026084339, -3.627061608673662008 ) ) ;
#7703 = DIRECTION ( 'NONE',  ( -0.000000000000000000, -0.000000000000000000, -1.000000000000000000 ) ) ;
#7704 = CARTESIAN_POINT ( 'NONE',  ( 27.29814976067589072, -3.294147343736874234, -8.283357778048660691 ) ) ;
#7705 = FACE_OUTER_BOUND ( 'NONE', #3215, .T. ) ;
#7706 = CARTESIAN_POINT ( 'NONE',  ( 26.31321956127059636, -7.341867041618697520, -6.247270588150510839 ) ) ;
#7707 = DIRECTION ( 'NONE',  ( -0.000000000000000000, -0.000000000000000000, 1.000000000000000000 ) ) ;
#7708 = ORIENTED_EDGE ( 'NONE', *, *, #7071, .F. ) ;
#7709 = EDGE_CURVE ( 'NONE', #11389, #17262, #10971, .T. ) ;
#7710 = CARTESIAN_POINT ( 'NONE',  ( 33.43363050022580296, -2.127845067243429256, -4.705209693361160461 ) ) ;
#7711 = CARTESIAN_POINT ( 'NONE',  ( 32.04575515724927470, -1.668086104879473730, -5.783357778048658915 ) ) ;
#7712 = ORIENTED_EDGE ( 'NONE', *, *, #15724, .F. ) ;
#7713 =( BOUNDED_CURVE ( )  B_SPLINE_CURVE ( 2, ( #16304, #9554, #15100, #12465, #1323, #12373, #11450, #14099, #4398 ),
 .UNSPECIFIED., .F., .T. ) 
 B_SPLINE_CURVE_WITH_KNOTS ( ( 3, 2, 2, 2, 3 ),
 ( 0.7115384615384615641, 0.7179487179487179516, 0.7307692307692307265, 0.7435897435897436125, 0.7500000000000000000 ),
 .UNSPECIFIED. ) 
 CURVE ( )  GEOMETRIC_REPRESENTATION_ITEM ( )  RATIONAL_B_SPLINE_CURVE ( ( 0.9330127018922194093, 0.9330127018922194093, 1.000000000000000000, 0.8660254037844387076, 1.000000000000000000, 0.8660254037844387076, 1.000000000000000000, 0.9330127018922194093, 0.9330127018922194093 ) ) 
 REPRESENTATION_ITEM ( '' )  );
#7714 = CARTESIAN_POINT ( 'NONE',  ( -13.00000000000000178, 1.592040838891559293E-15, -12.00000000000000000 ) ) ;
#7715 = DIRECTION ( 'NONE',  ( 0.1196152422706618645, -0.9928203230275510771, 0.000000000000000000 ) ) ;
#7716 = VERTEX_POINT ( 'NONE', #10724 ) ;
#7717 = CYLINDRICAL_SURFACE ( 'NONE', #14122, 2.500000000000001776 ) ;
#7718 = EDGE_CURVE ( 'NONE', #9693, #15182, #9635, .T. ) ;
#7719 = CARTESIAN_POINT ( 'NONE',  ( 32.79901970863393501, -6.593096864778464017, -5.783357778048668685 ) ) ;
#7720 = ORIENTED_EDGE ( 'NONE', *, *, #17594, .T. ) ;
#7721 = ORIENTED_EDGE ( 'NONE', *, *, #16962, .F. ) ;
#7722 = DIRECTION ( 'NONE',  ( 0.1195020427801297691, 0.9918807541847894926, 0.04349518650597275493 ) ) ;
#7723 = CARTESIAN_POINT ( 'NONE',  ( 33.52375369703867847, -2.544085015380856518, -8.283357778048660691 ) ) ;
#7724 = CARTESIAN_POINT ( 'NONE',  ( -19.43845002722867221, 2.988003976273734708, 0.000000000000000000 ) ) ;
#7725 = CARTESIAN_POINT ( 'NONE',  ( -2.749999999999988454, -20.49999999999999645, -13.00000000000000355 ) ) ;
#7726 = CARTESIAN_POINT ( 'NONE',  ( 31.80137159822941939, -6.386132006154467078, -4.533357778048668685 ) ) ;
#7727 = CARTESIAN_POINT ( 'NONE',  ( 26.47269060886452507, -6.728324053342490174, -6.861505862736166250 ) ) ;
#7728 = CARTESIAN_POINT ( 'NONE',  ( 26.00079723459025871, -4.771832887959356562, -3.592817407220987747 ) ) ;
#7729 = CARTESIAN_POINT ( 'NONE',  ( 31.68992120585416217, -1.700760206360153015, -5.783357778048664244 ) ) ;
#7730 = CARTESIAN_POINT ( 'NONE',  ( 11.20128062458870843, 15.41171339406673546, -16.67750984750043486 ) ) ;
#7731 = CARTESIAN_POINT ( 'NONE',  ( 29.54600080245929306, -4.477139269648729325, -3.283357778048664688 ) ) ;
#7732 = EDGE_CURVE ( 'NONE', #8890, #10810, #13561, .T. ) ;
#7733 =( BOUNDED_CURVE ( )  B_SPLINE_CURVE ( 3, ( #3926, #9438, #14978, #5352 ),
 .UNSPECIFIED., .F., .T. ) 
 B_SPLINE_CURVE_WITH_KNOTS ( ( 4, 4 ),
 ( 1.436990331221392081, 1.509167199807614601 ),
 .UNSPECIFIED. ) 
 CURVE ( )  GEOMETRIC_REPRESENTATION_ITEM ( )  RATIONAL_B_SPLINE_CURVE ( ( 1.000000000000000000, 0.9995659220841806025, 0.9995659220841806025, 1.000000000000000000 ) ) 
 REPRESENTATION_ITEM ( '' )  );
#7734 = CARTESIAN_POINT ( 'NONE',  ( 15.92260893619738837, -28.39189527176317540, 16.15082599432113142 ) ) ;
#7735 = ADVANCED_FACE ( 'NONE', ( #16297 ), #9377, .T. ) ;
#7736 = VERTEX_POINT ( 'NONE', #1137 ) ;
#7737 = DIRECTION ( 'NONE',  ( 0.7999999999999999334, -0.6000000000000001998, 0.000000000000000000 ) ) ;
#7738 = CARTESIAN_POINT ( 'NONE',  ( 26.92924972366625980, -7.310485091653801781, -5.783357778048657138 ) ) ;
#7739 = CARTESIAN_POINT ( 'NONE',  ( -9.750000000000035527, -3.897114317029883868, -3.000000000000002665 ) ) ;
#7740 = ORIENTED_EDGE ( 'NONE', *, *, #2146, .T. ) ;
#7741 = FACE_OUTER_BOUND ( 'NONE', #4767, .T. ) ;
#7742 = CARTESIAN_POINT ( 'NONE',  ( 3.248936832696172505, -15.16081378324841289, -17.00000000000000000 ) ) ;
#7743 = VECTOR ( 'NONE', #665, 1000.000000000000000 ) ;
#7744 = DIRECTION ( 'NONE',  ( -1.000000000000000000, 0.000000000000000000, 0.000000000000000000 ) ) ;
#7745 = CARTESIAN_POINT ( 'NONE',  ( 30.09392748191118017, -6.591845302810410701, -7.033357778048666908 ) ) ;
#7746 = PLANE ( 'NONE',  #4338 ) ;
#7747 = CONTEXT_DEPENDENT_SHAPE_REPRESENTATION ( #4372, #10393 ) ;
#7748 = DIRECTION ( 'NONE',  ( 0.000000000000000000, 0.000000000000000000, -1.000000000000000000 ) ) ;
#7749 = CARTESIAN_POINT ( 'NONE',  ( 31.03886041246737548, -3.043338102658604161, -3.627061608673662008 ) ) ;
#7750 = EDGE_CURVE ( 'NONE', #13433, #2203, #5292, .T. ) ;
#7751 = CARTESIAN_POINT ( 'NONE',  ( -20.25000000000000355, -16.21813761408365195, 0.000000000000000000 ) ) ;
#7752 = DIRECTION ( 'NONE',  ( 1.000000000000000000, 0.000000000000000000, 0.000000000000000000 ) ) ;
#7753 = CARTESIAN_POINT ( 'NONE',  ( 26.62577407660990758, -3.575027854551694695, 7.939653947423664704 ) ) ;
#7754 = AXIS2_PLACEMENT_3D ( 'NONE', #1944, #4644, #6091 ) ;
#7755 = VERTEX_POINT ( 'NONE', #4392 ) ;
#7756 = VERTEX_POINT ( 'NONE', #3038 ) ;
#7757 = CARTESIAN_POINT ( 'NONE',  ( 26.03917326857634151, -4.899642733102906433, 7.939653947423662039 ) ) ;
#7758 = CARTESIAN_POINT ( 'NONE',  ( -45.00000000000000711, -19.03270077640482683, -10.53798182577225084 ) ) ;
#7759 = CARTESIAN_POINT ( 'NONE',  ( 32.24155699611449677, -1.634298987580965923, -5.783357778048664244 ) ) ;
#7760 = ORIENTED_EDGE ( 'NONE', *, *, #4408, .F. ) ;
#7761 = CARTESIAN_POINT ( 'NONE',  ( 25.71748644841968456, -2.420320648352046078, -5.783357778048663356 ) ) ;
#7762 = ORIENTED_EDGE ( 'NONE', *, *, #5016, .F. ) ;
#7763 = CARTESIAN_POINT ( 'NONE',  ( 30.61177514885986639, -5.802548093181622235, 3.283357778048663356 ) ) ;
#7764 = EDGE_CURVE ( 'NONE', #9531, #15791, #8754, .T. ) ;
#7765 = EDGE_LOOP ( 'NONE', ( #776, #11827, #13808, #6151, #16615 ) ) ;
#7766 = ORIENTED_EDGE ( 'NONE', *, *, #10585, .F. ) ;
#7767 = FACE_OUTER_BOUND ( 'NONE', #778, .T. ) ;
#7768 = B_SPLINE_CURVE_WITH_KNOTS ( 'NONE', 3,
 ( #5948, #14037, #10024, #9843 ),
 .UNSPECIFIED., .F., .F.,
 ( 4, 4 ),
 ( 0.000000000000000000, 0.0003446252387907819490 ),
 .UNSPECIFIED. ) ;
#7769 = CARTESIAN_POINT ( 'NONE',  ( 32.29974222271236073, -2.891426744974864071, -3.627061608673662008 ) ) ;
#7770 = CARTESIAN_POINT ( 'NONE',  ( 32.54050588463559990, -2.235448945602741766, -6.861505862736159145 ) ) ;
#7771 = CARTESIAN_POINT ( 'NONE',  ( 31.35480929215617252, -6.439933945126671055, 4.533357778048659803 ) ) ;
#7772 = AXIS2_PLACEMENT_3D ( 'NONE', #12693, #8531, #190 ) ;
#7773 = CARTESIAN_POINT ( 'NONE',  ( 27.30005507882132676, -4.747731375419166788, -3.627061608673664672 ) ) ;
#7774 = EDGE_CURVE ( 'NONE', #6225, #3798, #5782, .T. ) ;
#7775 = FACE_BOUND ( 'NONE', #6210, .T. ) ;
#7776 = CARTESIAN_POINT ( 'NONE',  ( 33.50243880635947846, -1.482387629897225390, -5.783357778048663356 ) ) ;
#7777 = CARTESIAN_POINT ( 'NONE',  ( 5.200000000000002842, 3.306546357697854226E-16, 2.700000000000000622 ) ) ;
#7778 = CIRCLE ( 'NONE', #17934, 2.000000000000001776 ) ;
#7779 = CARTESIAN_POINT ( 'NONE',  ( 27.23057351405260818, -1.848475362037681480, 5.783357778048668685 ) ) ;
#7780 = ORIENTED_EDGE ( 'NONE', *, *, #7517, .F. ) ;
#7781 = ORIENTED_EDGE ( 'NONE', *, *, #15623, .F. ) ;
#7782 = AXIS2_PLACEMENT_3D ( 'NONE', #10296, #7686, #2346 ) ;
#7783 = ORIENTED_EDGE ( 'NONE', *, *, #14522, .F. ) ;
#7784 = CARTESIAN_POINT ( 'NONE',  ( 26.87106449706838873, -6.053357334259913181, 7.939653947423658487 ) ) ;
#7785 = DIRECTION ( 'NONE',  ( -0.7071067811865254793, 0.000000000000000000, 0.7071067811865695552 ) ) ;
#7786 = ORIENTED_EDGE ( 'NONE', *, *, #11266, .F. ) ;
#7787 = FILL_AREA_STYLE_COLOUR ( '', #5432 ) ;
#7788 = CARTESIAN_POINT ( 'NONE',  ( 33.76207435632690590, -3.969185667289998332, -3.627061608673664672 ) ) ;
#7789 = ADVANCED_FACE ( 'NONE', ( #12823 ), #14009, .F. ) ;
#7790 = CARTESIAN_POINT ( 'NONE',  ( 29.16815758536418102, -2.004582921727632971, -5.783357778048664244 ) ) ;
#7791 = CARTESIAN_POINT ( 'NONE',  ( 28.40332666278570173, -4.614808937445885384, -7.939653947423662039 ) ) ;
#7792 = CYLINDRICAL_SURFACE ( 'NONE', #1492, 5.000000000000001776 ) ;
#7793 = DIRECTION ( 'NONE',  ( 0.000000000000000000, 0.000000000000000000, 1.000000000000000000 ) ) ;
#7794 = CARTESIAN_POINT ( 'NONE',  ( 32.46178999037268653, -4.125844254797621957, -8.283357778048662468 ) ) ;
#7795 = DIRECTION ( 'NONE',  ( 0.000000000000000000, 0.000000000000000000, 1.000000000000000000 ) ) ;
#7796 = CARTESIAN_POINT ( 'NONE',  ( -35.77680296528374271, -19.03270077640483038, -0.5379818257722508434 ) ) ;
#7797 = CARTESIAN_POINT ( 'NONE',  ( 30.01512236704901682, -6.601339762873093875, -7.033357778048666908 ) ) ;
#7798 = CIRCLE ( 'NONE', #15320, 10.50000000000000000 ) ;
#7799 = CARTESIAN_POINT ( 'NONE',  ( 31.24031073583692475, -4.273008382657478954, -3.627061608673664672 ) ) ;
#7800 = EDGE_CURVE ( 'NONE', #6646, #16041, #17478, .T. ) ;
#7801 = CARTESIAN_POINT ( 'NONE',  ( 32.50119254608192421, -4.121097024973739309, -3.627061608673664672 ) ) ;
#7802 = EDGE_LOOP ( 'NONE', ( #16163, #16973, #8246, #3429 ) ) ;
#7803 = LINE ( 'NONE', #4984, #240 ) ;
#7804 = PRODUCT_RELATED_PRODUCT_CATEGORY ( 'part', '', ( #11993 ) ) ;
#7805 = LINE ( 'NONE', #17354, #13635 ) ;
#7806 = AXIS2_PLACEMENT_3D ( 'NONE', #5681, #12671, #7161 ) ;
#7807 = EDGE_LOOP ( 'NONE', ( #6405, #7294, #14683, #13994 ) ) ;
#7808 = CARTESIAN_POINT ( 'NONE',  ( 32.64557936882268052, -2.222789665795767089, -4.705209693361161349 ) ) ;
#7809 = ORIENTED_EDGE ( 'NONE', *, *, #9154, .T. ) ;
#7810 = AXIS2_PLACEMENT_3D ( 'NONE', #6102, #760, #11631 ) ;
#7811 = EDGE_CURVE ( 'NONE', #13145, #5285, #10084, .T. ) ;
#7812 = CARTESIAN_POINT ( 'NONE',  ( 27.92859066579839222, -3.218191664895003523, 3.283357778048666464 ) ) ;
#7813 = CARTESIAN_POINT ( 'NONE',  ( 30.98067518586950442, -1.786210345264705790, -5.783357778048658027 ) ) ;
#7814 = ADVANCED_FACE ( 'NONE', ( #7399 ), #14285, .F. ) ;
#7815 = CARTESIAN_POINT ( 'NONE',  ( 25.81704846941310194, -3.246696919197676223, 7.157325878379703354 ) ) ;
#7816 = CARTESIAN_POINT ( 'NONE',  ( -0.1404055950190654656, -4.699865361597007407, -3.386887224136973185 ) ) ;
#7817 = CARTESIAN_POINT ( 'NONE',  ( 31.27600417729400917, -6.449428405189353342, -7.033357778048666908 ) ) ;
#7818 = AXIS2_PLACEMENT_3D ( 'NONE', #11359, #16928, #4308 ) ;
#7819 = ORIENTED_EDGE ( 'NONE', *, *, #9237, .F. ) ;
#7820 = CARTESIAN_POINT ( 'NONE',  ( 27.49697864365563760, -2.843094376337701679, -6.861505862736159145 ) ) ;
#7821 = CARTESIAN_POINT ( 'NONE',  ( 8.632250723006720250, -18.84644399697197770, 13.00000000000000178 ) ) ;
#7822 = CARTESIAN_POINT ( 'NONE',  ( -15.92260893619738837, -28.39189527176317540, -0.000000000000000000 ) ) ;
#7823 = CARTESIAN_POINT ( 'NONE',  ( 33.76397967447234549, -5.422769698972272678, -8.283357778048664244 ) ) ;
#7824 = CARTESIAN_POINT ( 'NONE',  ( 27.38828526237195504, -6.917821758047558056, -4.533357778048668685 ) ) ;
#7825 = CARTESIAN_POINT ( 'NONE',  ( 31.28415083292585663, -5.521667582366822202, -3.627061608673667781 ) ) ;
#7826 = ORIENTED_EDGE ( 'NONE', *, *, #8540, .T. ) ;
#7827 = ORIENTED_EDGE ( 'NONE', *, *, #11232, .F. ) ;
#7828 = PLANE ( 'NONE',  #6892 ) ;
#7829 = DIRECTION ( 'NONE',  ( 0.1113444980252557837, -0.9937818688019538493, 0.000000000000000000 ) ) ;
#7830 = VERTEX_POINT ( 'NONE', #415 ) ;
#7831 = CARTESIAN_POINT ( 'NONE',  ( 26.08205926866326863, -5.446317154234561642, 3.408606443870483282 ) ) ;
#7832 = DIRECTION ( 'NONE',  ( -0.000000000000000000, -0.000000000000000000, 1.000000000000000000 ) ) ;
#7833 = AXIS2_PLACEMENT_3D ( 'NONE', #12779, #12417, #3001 ) ;
#7834 = EDGE_CURVE ( 'NONE', #625, #9800, #7103, .T. ) ;
#7835 = DIRECTION ( 'NONE',  ( 0.000000000000000000, 0.000000000000000000, -1.000000000000000000 ) ) ;
#7836 = ORIENTED_EDGE ( 'NONE', *, *, #10260, .T. ) ;
#7837 = DIRECTION ( 'NONE',  ( 0.000000000000000000, 0.000000000000000000, 1.000000000000000000 ) ) ;
#7838 =( BOUNDED_CURVE ( )  B_SPLINE_CURVE ( 2, ( #2886, #2797, #8695, #16765, #4336, #5593, #1540, #9941, #1815 ),
 .UNSPECIFIED., .F., .T. ) 
 B_SPLINE_CURVE_WITH_KNOTS ( ( 3, 2, 2, 2, 3 ),
 ( 0.3653846153846154188, 0.3717948717948718063, 0.3846153846153846367, 0.3974358974358974117, 0.4038461538461538547 ),
 .UNSPECIFIED. ) 
 CURVE ( )  GEOMETRIC_REPRESENTATION_ITEM ( )  RATIONAL_B_SPLINE_CURVE ( ( 0.9330127018922194093, 0.9330127018922196314, 1.000000000000000000, 0.8660254037844387076, 1.000000000000000000, 0.8660254037844387076, 1.000000000000000000, 0.9330127018922190762, 0.9330127018922194093 ) ) 
 REPRESENTATION_ITEM ( '' )  );
#7839 = CARTESIAN_POINT ( 'NONE',  ( 28.86683379497783264, -7.466592651343750831, -5.783357778048669573 ) ) ;
#7840 = CARTESIAN_POINT ( 'NONE',  ( 23.02601376483258022, 3.965314980223224151, 0.000000000000000000 ) ) ;
#7841 = AXIS2_PLACEMENT_3D ( 'NONE', #8188, #12436, #2480 ) ;
#7842 = EDGE_CURVE ( 'NONE', #6854, #2179, #4480, .T. ) ;
#7843 = ITEM_DEFINED_TRANSFORMATION ( 'NONE', 'NONE', #13196,  #3575 ) ;
#7844 = DIRECTION ( 'NONE',  ( -0.000000000000000000, 1.000000000000000000, -0.000000000000000000 ) ) ;
#7845 = FACE_OUTER_BOUND ( 'NONE', #2971, .T. ) ;
#7846 = CIRCLE ( 'NONE', #8711, 2.000000000000001776 ) ;
#7847 = CARTESIAN_POINT ( 'NONE',  ( 29.56783163384821833, -3.220568019956291383, -7.939653947423660263 ) ) ;
#7848 = CARTESIAN_POINT ( 'NONE',  ( 33.28924367748503244, -4.026152426421394814, -7.939653947423662039 ) ) ;
#7849 = CARTESIAN_POINT ( 'NONE',  ( 28.77507474356526984, -18.63405514100518801, -13.50648245236009792 ) ) ;
#7850 = CARTESIAN_POINT ( 'NONE',  ( 25.99533317148741318, -3.650983533393564517, 7.939653947423664704 ) ) ;
#7851 = AXIS2_PLACEMENT_3D ( 'NONE', #1750, #1383, #9880 ) ;
#7852 = STYLED_ITEM ( 'NONE', ( #10026 ), #14616 ) ;
#7853 = ORIENTED_EDGE ( 'NONE', *, *, #5162, .T. ) ;
#7854 = CARTESIAN_POINT ( 'NONE',  ( 28.91547068018125799, -2.672194098943493135, 4.705209693361168455 ) ) ;
#7855 = CARTESIAN_POINT ( 'NONE',  ( 27.21934464581372737, -3.303641803799556964, -8.283357778048660691 ) ) ;
#7856 = ORIENTED_EDGE ( 'NONE', *, *, #15285, .F. ) ;
#7857 = AXIS2_PLACEMENT_3D ( 'NONE', #6534, #9417, #7715 ) ;
#7858 = DIRECTION ( 'NONE',  ( -0.000000000000000000, -0.000000000000000000, -1.000000000000000000 ) ) ;
#7859 = CARTESIAN_POINT ( 'NONE',  ( 30.63309003953906995, -6.864245478665264244, 5.783357778048664244 ) ) ;
#7860 = ADVANCED_FACE ( 'NONE', ( #12552 ), #15734, .F. ) ;
#7861 = DIRECTION ( 'NONE',  ( -0.8660254037844363761, 0.5000000000000038858, 0.000000000000000000 ) ) ;
#7862 = CARTESIAN_POINT ( 'NONE',  ( 32.95662993491455950, -6.574107945067995118, -5.783357778048669573 ) ) ;
#7863 = VECTOR ( 'NONE', #8313, 1000.000000000000227 ) ;
#7864 = CARTESIAN_POINT ( 'NONE',  ( 32.77709966008947617, -5.968767264923789284, -6.861505862736166250 ) ) ;
#7865 = CARTESIAN_POINT ( 'NONE',  ( 28.44643833274707845, -2.428894455266221275, -7.033357778048658027 ) ) ;
#7866 = DIRECTION ( 'NONE',  ( 0.7999999999999999334, 0.6000000000000001998, 0.000000000000000000 ) ) ;
#7867 = CARTESIAN_POINT ( 'NONE',  ( 30.10960860451258370, -6.927314653643411368, -6.453230759126470595 ) ) ;
#7868 = EDGE_CURVE ( 'NONE', #133, #11061, #15635, .T. ) ;
#7869 = CARTESIAN_POINT ( 'NONE',  ( -8.632250723006722026, -18.84644399697197770, 16.84735068286508763 ) ) ;
#7870 = CARTESIAN_POINT ( 'NONE',  ( 27.50829672905005907, -3.268828784122926212, -3.283357778048662023 ) ) ;
#7871 = CARTESIAN_POINT ( 'NONE',  ( 26.75784435724945709, -6.993777436889428323, -4.533357778048668685 ) ) ;
#7872 = CARTESIAN_POINT ( 'NONE',  ( 28.86683379497783264, -7.466592651343750831, 5.783357778048657138 ) ) ;
#7873 = VERTEX_POINT ( 'NONE', #12726 ) ;
#7874 = ORIENTED_EDGE ( 'NONE', *, *, #7106, .F. ) ;
#7875 = AXIS2_PLACEMENT_3D ( 'NONE', #9446, #12350, #2484 ) ;
#7876 = CIRCLE ( 'NONE', #7595, 1.000000000000000000 ) ;
#7877 = ORIENTED_EDGE ( 'NONE', *, *, #14911, .T. ) ;
#7878 = CARTESIAN_POINT ( 'NONE',  ( 32.97402322492378346, -4.064130265842336165, 7.939653947423662039 ) ) ;
#7879 = CARTESIAN_POINT ( 'NONE',  ( 31.56875459193803124, -6.114348982704044921, 6.861505862736157368 ) ) ;
#7880 = EDGE_LOOP ( 'NONE', ( #17660, #1978 ) ) ;
#7881 = DIRECTION ( 'NONE',  ( -0.6674414130531752809, 0.7446623128248003320, -9.100287414781897985E-16 ) ) ;
#7882 = DIRECTION ( 'NONE',  ( 0.000000000000000000, 0.000000000000000000, -1.000000000000000000 ) ) ;
#7883 = CARTESIAN_POINT ( 'NONE',  ( 26.01652455409633902, -4.902371455920926380, 5.783357778048663356 ) ) ;
#7885 = VECTOR ( 'NONE', #16755, 1000.000000000000227 ) ;
#7884 = CARTESIAN_POINT ( 'NONE',  ( 29.80442540930208750, -6.953886339277345563, -5.783357778048669573 ) ) ;
#7886 = CARTESIAN_POINT ( 'NONE',  ( 28.55903157092087952, -3.142235986053133256, -8.283357778048660691 ) ) ;
#7887 = DIRECTION ( 'NONE',  ( -1.000000000000000000, -1.224646799147353454E-16, 0.000000000000000000 ) ) ;
#7888 = DIRECTION ( 'NONE',  ( 0.000000000000000000, 0.000000000000000000, -1.000000000000000000 ) ) ;
#7889 = DIRECTION ( 'NONE',  ( 1.000000000000000000, 1.776356839400250465E-15, 0.000000000000000000 ) ) ;
#7890 = DIRECTION ( 'NONE',  ( 4.179998415399335043E-17, -3.469446951953615175E-16, -1.000000000000000000 ) ) ;
#7891 = AXIS2_PLACEMENT_3D ( 'NONE', #9169, #6541, #13343 ) ;
#7892 = CARTESIAN_POINT ( 'NONE',  ( 30.78487334700428590, -1.819997462563214263, -5.783357778048658027 ) ) ;
#7893 = CARTESIAN_POINT ( 'NONE',  ( 33.32855701603872234, -2.140504347050403045, -6.861505862736158257 ) ) ;
#7894 = EDGE_LOOP ( 'NONE', ( #10062, #14436, #17532, #1049 ) ) ;
#7895 = CARTESIAN_POINT ( 'NONE',  ( 31.97277696464621854, -6.702839660918840536, 5.783357778048664244 ) ) ;
#7896 = ADVANCED_FACE ( 'NONE', ( #11158 ), #1592, .T. ) ;
#7897 = CARTESIAN_POINT ( 'NONE',  ( -7.666200962222251114, 6.158133996769793228, -2.333128398347828369 ) ) ;
#7898 = AXIS2_PLACEMENT_3D ( 'NONE', #15360, #9633, #8285 ) ;
#7899 = ORIENTED_EDGE ( 'NONE', *, *, #7709, .T. ) ;
#7900 = DIRECTION ( 'NONE',  ( -0.1196152422706610735, 0.9928203230275511881, 0.000000000000000000 ) ) ;
#7901 = CARTESIAN_POINT ( 'NONE',  ( 29.38830135902312080, -2.615227339812091767, -6.861505862736159145 ) ) ;
#7902 = EDGE_CURVE ( 'NONE', #17331, #5257, #3308, .T. ) ;
#7903 = CARTESIAN_POINT ( 'NONE',  ( 27.89480254248674740, -2.495355674045408367, 4.533357778048667797 ) ) ;
#7904 = CARTESIAN_POINT ( 'NONE',  ( 30.96820195323705605, -2.125071739898741097, -7.033357778048658027 ) ) ;
#7905 = CARTESIAN_POINT ( 'NONE',  ( 27.90727577511918867, -2.156494279411373061, -5.783357778048670461 ) ) ;
#7906 = DIRECTION ( 'NONE',  ( 5.026720092345836698E-22, -4.581671729415424240E-22, 1.000000000000000000 ) ) ;
#7907 = CARTESIAN_POINT ( 'NONE',  ( 33.20111501597313719, -6.944397359513344803, -5.783357778048669573 ) ) ;
#7908 = CARTESIAN_POINT ( 'NONE',  ( 32.54503264317084188, -5.369756224683081669, -3.627061608673667781 ) ) ;
#7909 = DIRECTION ( 'NONE',  ( 1.000000000000000000, 0.000000000000000000, 0.000000000000000000 ) ) ;
#7910 = CARTESIAN_POINT ( 'NONE',  ( 31.92138306490751987, -2.737139032229836566, -3.283357778048662023 ) ) ;
#7911 = CARTESIAN_POINT ( 'NONE',  ( 15.39462056267347734, 12.71537873815137232, -16.22282132715419678 ) ) ;
#7912 = CARTESIAN_POINT ( 'NONE',  ( 39.19942832275109623, -5.640193629429878897, -9.783357778048662468 ) ) ;
#7913 = EDGE_CURVE ( 'NONE', #16382, #7391, #10268, .T. ) ;
#7914 = CARTESIAN_POINT ( 'NONE',  ( 30.78070346053490880, -6.209293581256383199, -4.705209693361168455 ) ) ;
#7915 = EDGE_CURVE ( 'NONE', #15856, #12531, #5736, .T. ) ;
#7916 = AXIS2_PLACEMENT_3D ( 'NONE', #7244, #10025, #8867 ) ;
#7917 = VERTEX_POINT ( 'NONE', #3483 ) ;
#7918 = CIRCLE ( 'NONE', #14872, 13.00000000000000178 ) ;
#7919 = ORIENTED_EDGE ( 'NONE', *, *, #4365, .T. ) ;
#7920 = DIRECTION ( 'NONE',  ( -0.8243186046180107640, -0.5661261679878573094, -0.000000000000000000 ) ) ;
#7921 = CARTESIAN_POINT ( 'NONE',  ( -29.25000000000000000, -15.80023397548365871, -13.37255996287876592 ) ) ;
#7922 = VECTOR ( 'NONE', #3162, 1000.000000000000114 ) ;
#7923 = ORIENTED_EDGE ( 'NONE', *, *, #13451, .T. ) ;
#7924 = DIRECTION ( 'NONE',  ( 0.1196152422706596996, -0.9928203230275514102, 0.000000000000000000 ) ) ;
#7925 =( BOUNDED_CURVE ( )  B_SPLINE_CURVE ( 2, ( #9249, #8900, #17455, #2383, #3458, #16161, #737, #16076, #822 ),
 .UNSPECIFIED., .F., .T. ) 
 B_SPLINE_CURVE_WITH_KNOTS ( ( 3, 2, 2, 2, 3 ),
 ( 0.8653846153846154188, 0.8717948717948718063, 0.8846153846153845812, 0.8974358974358974672, 0.9012882778258578531 ),
 .UNSPECIFIED. ) 
 CURVE ( )  GEOMETRIC_REPRESENTATION_ITEM ( )  RATIONAL_B_SPLINE_CURVE ( ( 0.9330127018922192983, 0.9330127018922198534, 1.000000000000000000, 0.8660254037844387076, 1.000000000000000000, 0.8660254037844387076, 1.000000000000000000, 0.9597425536373320742, 0.9436786787937823107 ) ) 
 REPRESENTATION_ITEM ( '' )  );
#7927 = ORIENTED_EDGE ( 'NONE', *, *, #14584, .F. ) ;
#7926 = PLANE ( 'NONE',  #9028 ) ;
#7928 = CARTESIAN_POINT ( 'NONE',  ( 32.67619606237177265, -1.592130426037604352, -5.783357778048658915 ) ) ;
#7929 = DIRECTION ( 'NONE',  ( 5.615616396709274052E-18, -4.661026453772598353E-17, -1.000000000000000000 ) ) ;
#7930 = ORIENTED_EDGE ( 'NONE', *, *, #1916, .T. ) ;
#7931 = CARTESIAN_POINT ( 'NONE',  ( 33.40754056521197413, -5.892811586081919906, -6.861505862736166250 ) ) ;
#7932 = CARTESIAN_POINT ( 'NONE',  ( 0.000000000000000000, 0.000000000000000000, -8.700000000000001066 ) ) ;
#7933 = CYLINDRICAL_SURFACE ( 'NONE', #1663, 2.499999999999999112 ) ;
#7934 = CARTESIAN_POINT ( 'NONE',  ( 29.55043834383899437, -5.730545699181964991, -3.627061608673668225 ) ) ;
#7935 = CARTESIAN_POINT ( 'NONE',  ( 5.000000000000000888, 4.250000000000000000, 0.000000000000000000 ) ) ;
#7936 = CARTESIAN_POINT ( 'NONE',  ( 30.58169613980036772, -2.898544849976259385, 8.283357778048664244 ) ) ;
#7937 = EDGE_LOOP ( 'NONE', ( #9437, #6048, #10634, #11925 ) ) ;
#7938 = EDGE_CURVE ( 'NONE', #16655, #12357, #14464, .T. ) ;
#7939 = ORIENTED_EDGE ( 'NONE', *, *, #2831, .T. ) ;
#7940 = CARTESIAN_POINT ( 'NONE',  ( 30.19827253897071273, -3.144612341114420673, 3.627061608673666893 ) ) ;
#7941 = LINE ( 'NONE', #9459, #5792 ) ;
#7942 = DIRECTION ( 'NONE',  ( -1.000000000000000000, 0.000000000000000000, 0.000000000000000000 ) ) ;
#7943 = EDGE_CURVE ( 'NONE', #15452, #3773, #6857, .T. ) ;
#7944 = ORIENTED_EDGE ( 'NONE', *, *, #3467, .F. ) ;
#7945 =( LENGTH_UNIT ( ) NAMED_UNIT ( * ) SI_UNIT ( .MILLI., .METRE. ) );
#7946 = EDGE_LOOP ( 'NONE', ( #11758, #4339, #1555, #2086, #11320 ) ) ;
#7947 = DIRECTION ( 'NONE',  ( 1.000000000000000000, 0.000000000000000000, 0.000000000000000000 ) ) ;
#7948 =( BOUNDED_CURVE ( )  B_SPLINE_CURVE ( 2, ( #12595, #2995, #15499, #5686, #11201, #13861, #6977, #3080, #1448 ),
 .UNSPECIFIED., .F., .T. ) 
 B_SPLINE_CURVE_WITH_KNOTS ( ( 3, 2, 2, 2, 3 ),
 ( 0.5961538461538461453, 0.6025641025641025328, 0.6153846153846154188, 0.6282051282051281937, 0.6346153846153846922 ),
 .UNSPECIFIED. ) 
 CURVE ( )  GEOMETRIC_REPRESENTATION_ITEM ( )  RATIONAL_B_SPLINE_CURVE ( ( 0.9330127018922194093, 0.9330127018922194093, 1.000000000000000000, 0.8660254037844387076, 1.000000000000000000, 0.8660254037844387076, 1.000000000000000000, 0.9330127018922187432, 0.9330127018922192983 ) ) 
 REPRESENTATION_ITEM ( '' )  );
#7949 = CARTESIAN_POINT ( 'NONE',  ( -1.917618200156724081E-28, -7.000000000000001776, 0.000000000000000000 ) ) ;
#7950 = CARTESIAN_POINT ( 'NONE',  ( 28.71854711534694715, -4.576831098024959132, -3.627061608673664672 ) ) ;
#7951 = CARTESIAN_POINT ( 'NONE',  ( 15.92260893619738837, -28.39189527176317540, 6.000000000000000000 ) ) ;
#7952 = CARTESIAN_POINT ( 'NONE',  ( 26.23609683341064525, -2.995005734021441768, 4.705209693361167567 ) ) ;
#7953 = PRODUCT_DEFINITION_SHAPE ( 'NONE', 'NONE',  #17975 ) ;
#7954 = ORIENTED_EDGE ( 'NONE', *, *, #17702, .F. ) ;
#7955 = CARTESIAN_POINT ( 'NONE',  ( -45.50000000000000000, -16.03270077640482683, -8.287981825772241962 ) ) ;
#7956 = CARTESIAN_POINT ( 'NONE',  ( 32.38298487551052318, -4.135338714860305132, 3.283357778048664244 ) ) ;
#7957 = CARTESIAN_POINT ( 'NONE',  ( 32.43181250335191379, -6.310176327312596811, -4.533357778048668685 ) ) ;
#7958 = CARTESIAN_POINT ( 'NONE',  ( 27.60595198473284384, -7.618504009027492252, 5.783357778048657138 ) ) ;
#7959 = ADVANCED_FACE ( 'NONE', ( #13186, #4827 ), #14565, .F. ) ;
#7960 = VERTEX_POINT ( 'NONE', #764 ) ;
#7961 = ORIENTED_EDGE ( 'NONE', *, *, #7517, .T. ) ;
#7962 = ORIENTED_EDGE ( 'NONE', *, *, #5877, .F. ) ;
#7963 = ORIENTED_EDGE ( 'NONE', *, *, #3605, .T. ) ;
#7964 = CARTESIAN_POINT ( 'NONE',  ( 32.65880277236253448, -4.102108105263264193, 3.627061608673664228 ) ) ;
#7965 = CARTESIAN_POINT ( 'NONE',  ( 31.69574812466957781, -6.726019302751734763, 5.783357778048657138 ) ) ;
#7966 = EDGE_CURVE ( 'NONE', #9791, #2265, #14646, .T. ) ;
#7967 = VERTEX_POINT ( 'NONE', #6288 ) ;
#7968 = CARTESIAN_POINT ( 'NONE',  ( -11.73134587110777005, -4.864722402403119261, -9.600000000000001421 ) ) ;
#7969 = CARTESIAN_POINT ( 'NONE',  ( 30.09392748191118017, -6.591845302810410701, -7.033357778048666908 ) ) ;
#7970 = CARTESIAN_POINT ( 'NONE',  ( 4.197393957002304887, 7.725818140447171444E-14, -3.203767560748932208 ) ) ;
#7971 = CARTESIAN_POINT ( 'NONE',  ( 27.88665588685489993, -3.423116496867954162, -3.627061608673662008 ) ) ;
#7972 = CARTESIAN_POINT ( 'NONE',  ( 28.19013153391124860, -7.158573733970061248, -5.783357778048657138 ) ) ;
#7973 = CARTESIAN_POINT ( 'NONE',  ( 31.67744797322171735, -2.039621600994187656, -7.033357778048658027 ) ) ;
#7974 = DIRECTION ( 'NONE',  ( -0.000000000000000000, -0.000000000000000000, -1.000000000000000000 ) ) ;
#7975 = DIRECTION ( 'NONE',  ( 0.000000000000000000, -0.4999999999999992228, 0.8660254037844390407 ) ) ;
#7976 = CARTESIAN_POINT ( 'NONE',  ( 29.98133424373737199, -5.878503772023492502, -8.283357778048664244 ) ) ;
#7977 = CARTESIAN_POINT ( 'NONE',  ( 32.81641299864316608, -4.083119185552795294, -7.939653947423662039 ) ) ;
#7978 = CARTESIAN_POINT ( 'NONE',  ( 33.58707084003705745, -6.498152266226124851, -5.783357778048669573 ) ) ;
#7979 = EDGE_LOOP ( 'NONE', ( #7780, #4276, #17656, #14589, #16002 ) ) ;
#7980 = CARTESIAN_POINT ( 'NONE',  ( -35.74085044863416272, -23.57886868891566223, 11.27079897466147607 ) ) ;
#7981 = EDGE_CURVE ( 'NONE', #3342, #7401, #8593, .T. ) ;
#7982 = DIRECTION ( 'NONE',  ( 0.9928203230275510771, 0.1196152422706609902, 4.006172263299092517E-17 ) ) ;
#7983 = AXIS2_PLACEMENT_3D ( 'NONE', #3953, #1146, #12201 ) ;
#7984 = ORIENTED_EDGE ( 'NONE', *, *, #2645, .T. ) ;
#7985 = CARTESIAN_POINT ( 'NONE',  ( 32.56242593318006584, -2.859778545457409837, 3.627061608673666449 ) ) ;
#7986 = CARTESIAN_POINT ( 'NONE',  ( 29.39282811755836988, -5.749534618892433002, -3.627061608673667781 ) ) ;
#7987 = LINE ( 'NONE', #16426, #3811 ) ;
#7988 = DIRECTION ( 'NONE',  ( 0.9928203230275510771, 0.1196152422706609902, 4.006172263299092517E-17 ) ) ;
#7989 = CARTESIAN_POINT ( 'NONE',  ( 33.48062616923409962, 0.02583177435455490112, -5.783357778048662468 ) ) ;
#7990 = DIRECTION ( 'NONE',  ( -0.000000000000000000, -0.000000000000000000, -1.000000000000000000 ) ) ;
#7991 = EDGE_CURVE ( 'NONE', #13453, #10591, #613, .T. ) ;
#7992 = CARTESIAN_POINT ( 'NONE',  ( 31.90644508241650357, -6.373472726347483963, -7.033357778048666908 ) ) ;
#7993 = CARTESIAN_POINT ( 'NONE',  ( 8.472608240843633681E-22, -7.722472891792491889E-22, -7.794427190999915211 ) ) ;
#7994 = CARTESIAN_POINT ( 'NONE',  ( 35.77680296528374271, -19.03270077640483038, 0.5379818257722508434 ) ) ;
#7995 = CARTESIAN_POINT ( 'NONE',  ( 31.78252145740879797, -2.026962321187214311, -4.533357778048659803 ) ) ;
#7996 = DIRECTION ( 'NONE',  ( -1.000000000000000000, 0.000000000000000000, 0.000000000000000000 ) ) ;
#7997 = CARTESIAN_POINT ( 'NONE',  ( -1.390214784104961021, -4.043996922316171805, -3.202509183706246265 ) ) ;
#7998 = ORIENTED_EDGE ( 'NONE', *, *, #1585, .F. ) ;
#7999 = CARTESIAN_POINT ( 'NONE',  ( 32.02836186724004364, -4.178063784105134459, -7.939653947423662039 ) ) ;
#8000 = CARTESIAN_POINT ( 'NONE',  ( 39.19942832275109623, -5.640193629429882449, -2.283357778048670461 ) ) ;
#8001 = CARTESIAN_POINT ( 'NONE',  ( -4.000000000000000000, -2.309401076758508253, -3.133295621305383083 ) ) ;
#8002 = ORIENTED_EDGE ( 'NONE', *, *, #8443, .F. ) ;
#8003 = CARTESIAN_POINT ( 'NONE',  ( 26.03655646321512052, -5.068638614726477698, 3.378836190363221803 ) ) ;
#8004 = CARTESIAN_POINT ( 'NONE',  ( 25.71748644841968456, -2.420320648352051851, -5.783357778048663356 ) ) ;
#8005 = ADVANCED_FACE ( 'NONE', ( #3584 ), #586, .T. ) ;
#8006 = CARTESIAN_POINT ( 'NONE',  ( 0.000000000000000000, 0.000000000000000000, 8.700000000000001066 ) ) ;
#8007 = ORIENTED_EDGE ( 'NONE', *, *, #16942, .T. ) ;
#8008 = CARTESIAN_POINT ( 'NONE',  ( 26.90793483298706690, -6.248787706170159773, -8.283357778048662468 ) ) ;
#8009 = CARTESIAN_POINT ( 'NONE',  ( 4.000000000000004441, -2.309401076758508697, -3.204271511726787924 ) ) ;
#8010 = DIRECTION ( 'NONE',  ( -1.000000000000000000, 0.000000000000000000, 0.000000000000000000 ) ) ;
#8011 = CARTESIAN_POINT ( 'NONE',  ( 26.49878054387835746, -2.963357534503999968, -4.705209693361160461 ) ) ;
#8012 = DIRECTION ( 'NONE',  ( 0.000000000000000000, 0.000000000000000000, 1.000000000000000000 ) ) ;
#8013 = ADVANCED_FACE ( 'NONE', ( #4153 ), #9398, .T. ) ;
#8014 = CARTESIAN_POINT ( 'NONE',  ( 31.00199007654869732, -2.847907730748336252, 3.283357778048666464 ) ) ;
#8015 = AXIS2_PLACEMENT_3D ( 'NONE', #2488, #13469, #13549 ) ;
#8016 = CARTESIAN_POINT ( 'NONE',  ( 28.40332666278570173, -4.614808937445885384, 3.627061608673664228 ) ) ;
#8017 = SURFACE_SIDE_STYLE ('',( #2494 ) ) ;
#8018 = CARTESIAN_POINT ( 'NONE',  ( 22.62413451274595388, -22.47014588436322668, 15.00416998627796694 ) ) ;
#8019 = ORIENTED_EDGE ( 'NONE', *, *, #16397, .T. ) ;
#8020 = CARTESIAN_POINT ( 'NONE',  ( -10.47816170930907553, 0.6768509389586230274, -6.005572809000082835 ) ) ;
#8021 = VERTEX_POINT ( 'NONE', #2518 ) ;
#8022 = CARTESIAN_POINT ( 'NONE',  ( 45.50000000000000000, -16.03270077640482683, 8.287981825772241962 ) ) ;
#8023 = ADVANCED_FACE ( 'NONE', ( #16320 ), #9482, .F. ) ;
#8024 = EDGE_LOOP ( 'NONE', ( #2455, #3053 ) ) ;
#8025 = DIRECTION ( 'NONE',  ( 0.9928203230275511881, 0.1196152422706614482, 0.000000000000000000 ) ) ;
#8026 = CARTESIAN_POINT ( 'NONE',  ( 29.02054416436834217, -2.659534819136519790, -4.705209693361160461 ) ) ;
#8027 = CIRCLE ( 'NONE', #216, 0.2000000000000000944 ) ;
#8028 = PRODUCT_DEFINITION_FORMATION_WITH_SPECIFIED_SOURCE ( 'ANY', '', #6352, .NOT_KNOWN. ) ;
#8029 = FACE_OUTER_BOUND ( 'NONE', #3768, .T. ) ;
#8030 = CARTESIAN_POINT ( 'NONE',  ( 27.93543013035303701, -2.153102235610331316, -5.113484796970857893 ) ) ;
#8031 = DIRECTION ( 'NONE',  ( -1.000000000000000000, 0.000000000000000000, 0.000000000000000000 ) ) ;
#8032 = CARTESIAN_POINT ( 'NONE',  ( 27.08121146544255353, -6.028038774645947839, 3.627061608673662896 ) ) ;
#8033 = CARTESIAN_POINT ( 'NONE',  ( 28.13194630731337753, -5.901445976576171759, 7.939653947423658487 ) ) ;
#8034 = AXIS2_PLACEMENT_3D ( 'NONE', #15528, #17186, #573 ) ;
#8035 = CARTESIAN_POINT ( 'NONE',  ( 8.632250723006720250, -18.84644399697197770, 16.84735068286506987 ) ) ;
#8036 = CARTESIAN_POINT ( 'NONE',  ( 32.53688598753899441, -6.297517047505613697, 4.533357778048659803 ) ) ;
#8037 = CARTESIAN_POINT ( 'NONE',  ( 33.58707084003705745, -6.498152266226123963, 5.783357778048657138 ) ) ;
#8038 = CARTESIAN_POINT ( 'NONE',  ( 26.87785582392756467, -3.344784462964796479, 8.283357778048664244 ) ) ;
#8039 = ORIENTED_EDGE ( 'NONE', *, *, #1700, .F. ) ;
#8040 = ORIENTED_EDGE ( 'NONE', *, *, #5177, .T. ) ;
#8041 = EDGE_LOOP ( 'NONE', ( #13363, #1443, #13774, #16870 ) ) ;
#8042 = CARTESIAN_POINT ( 'NONE',  ( 31.30154412293507349, -3.011689903141150815, 3.627061608673666893 ) ) ;
#8043 = DIRECTION ( 'NONE',  ( 0.000000000000000000, 0.000000000000000000, 1.000000000000000000 ) ) ;
#8044 = CARTESIAN_POINT ( 'NONE',  ( 31.06530721954707985, -6.801974981593605918, 5.783357778048657138 ) ) ;
#8045 = ORIENTED_EDGE ( 'NONE', *, *, #8272, .F. ) ;
#8046 = CARTESIAN_POINT ( 'NONE',  ( 30.48043329534786849, -5.818372192732907067, 8.283357778048660691 ) ) ;
#8047 = STYLED_ITEM ( 'NONE', ( #11952 ), #5266 ) ;
#8048 = CYLINDRICAL_SURFACE ( 'NONE', #6060, 5.500000000000000888 ) ;
#8049 = CARTESIAN_POINT ( 'NONE',  ( 26.01652455409633902, -4.902371455920926380, 5.783357778048663356 ) ) ;
#8050 = CARTESIAN_POINT ( 'NONE',  ( 28.52162355051263987, -6.481468097106410475, -6.861505862736167138 ) ) ;
#8051 = CARTESIAN_POINT ( 'NONE',  ( 4.281152949374505745, -4.203775615332239646, -2.000000000000000000 ) ) ;
#8053 = EDGE_CURVE ( 'NONE', #2135, #9636, #16569, .T. ) ;
#8052 = CARTESIAN_POINT ( 'NONE',  ( 33.24613200752366282, -6.212066908601060256, -7.033357778048666908 ) ) ;
#8054 = DIRECTION ( 'NONE',  ( 0.9928203230275512992, 0.1196152422706610180, 4.006172263299093133E-17 ) ) ;
#8055 = CARTESIAN_POINT ( 'NONE',  ( 1.393927851585477828, -4.043713361053538513, -3.226374918436841099 ) ) ;
#8056 = CYLINDRICAL_SURFACE ( 'NONE', #2699, 25.00000000000000000 ) ;
#8057 =( NAMED_UNIT ( * ) PLANE_ANGLE_UNIT ( ) SI_UNIT ( $, .RADIAN. ) );
#8058 = AXIS2_PLACEMENT_3D ( 'NONE', #8812, #646, #17450 ) ;
#8059 = CARTESIAN_POINT ( 'NONE',  ( 32.93470988637010066, -5.949778345213319497, -6.861505862736167138 ) ) ;
#8060 = EDGE_CURVE ( 'NONE', #4820, #16771, #10479, .T. ) ;
#8061 = CARTESIAN_POINT ( 'NONE',  ( 27.78610916120306129, -6.570083055755264745, -4.705209693361169343 ) ) ;
#8062 = DIRECTION ( 'NONE',  ( 0.000000000000000000, 0.000000000000000000, -1.000000000000000000 ) ) ;
#8063 = VECTOR ( 'NONE', #14116, 1000.000000000000000 ) ;
#8064 = CARTESIAN_POINT ( 'NONE',  ( 3.538288549924106796, -15.34800872113743431, -16.99955934415557479 ) ) ;
#8065 = AXIS2_PLACEMENT_3D ( 'NONE', #3134, #8848, #7582 ) ;
#8066 = VERTEX_POINT ( 'NONE', #1423 ) ;
#8067 = ORIENTED_EDGE ( 'NONE', *, *, #4609, .F. ) ;
#8068 = CARTESIAN_POINT ( 'NONE',  ( 32.77257290155422709, -2.834459985843462260, 7.939653947423662927 ) ) ;
#8069 = CARTESIAN_POINT ( 'NONE',  ( 28.12741954877813555, -2.767138697495831856, -6.861505862736159145 ) ) ;
#8070 = DIRECTION ( 'NONE',  ( 0.000000000000000000, 0.000000000000000000, 1.000000000000000000 ) ) ;
#8071 = DIRECTION ( 'NONE',  ( -1.000000000000000000, -0.000000000000000000, -0.000000000000000000 ) ) ;
#8072 = CARTESIAN_POINT ( 'NONE',  ( 28.74176732417158320, -7.092112515190875044, -5.783357778048657138 ) ) ;
#8073 = DIRECTION ( 'NONE',  ( -1.000000000000000000, -0.000000000000000000, -0.000000000000000000 ) ) ;
#8074 = VECTOR ( 'NONE', #5915, 1000.000000000000227 ) ;
#8075 = EDGE_CURVE ( 'NONE', #9144, #14530, #9887, .T. ) ;
#8076 = DIRECTION ( 'NONE',  ( 0.6000000000000000888, -0.7999999999999999334, 0.000000000000000000 ) ) ;
#8077 = CARTESIAN_POINT ( 'NONE',  ( 31.43732351782677625, -4.249272233123119413, -3.283357778048664688 ) ) ;
#8078 = ORIENTED_EDGE ( 'NONE', *, *, #6464, .T. ) ;
#8079 = VERTEX_POINT ( 'NONE', #5395 ) ;
#8080 = DIRECTION ( 'NONE',  ( -1.000000000000000000, 0.000000000000000000, 0.000000000000000000 ) ) ;
#8081 = EDGE_CURVE ( 'NONE', #2247, #17429, #11045, .T. ) ;
#8082 = DIRECTION ( 'NONE',  ( -0.000000000000000000, -0.000000000000000000, -1.000000000000000000 ) ) ;
#8083 = CARTESIAN_POINT ( 'NONE',  ( 25.71748644841968456, -2.420320648352046078, 5.783357778048663356 ) ) ;
#8084 = CYLINDRICAL_SURFACE ( 'NONE', #8759, 2.500000000000001776 ) ;
#8085 = AXIS2_PLACEMENT_3D ( 'NONE', #15192, #11257, #1509 ) ;
#8086 = CARTESIAN_POINT ( 'NONE',  ( 26.86291784143654127, -6.981118157082444320, -7.033357778048666908 ) ) ;
#8087 = CARTESIAN_POINT ( 'NONE',  ( 32.75517961154501023, -5.344437665069116328, -7.939653947423662927 ) ) ;
#8088 = AXIS2_PLACEMENT_3D ( 'NONE', #70, #5582, #9738 ) ;
#8089 = EDGE_CURVE ( 'NONE', #17584, #15376, #11273, .T. ) ;
#8090 = DIRECTION ( 'NONE',  ( -0.000000000000000000, -0.000000000000000000, -1.000000000000000000 ) ) ;
#8091 = CARTESIAN_POINT ( 'NONE',  ( -28.60529878918911706, -13.42304697295875648, -13.55371198823188017 ) ) ;
#8092 = ORIENTED_EDGE ( 'NONE', *, *, #15855, .F. ) ;
#8093 = CARTESIAN_POINT ( 'NONE',  ( 26.18940075748478691, -6.337263906362392341, 3.743184633113769699 ) ) ;
#8094 = CIRCLE ( 'NONE', #5182, 5.500000000000000000 ) ;
#8095 = PRODUCT ( 'o-rings series g_iso_O-ring 23.6x1.8-B-ISO 3601-1', 'o-rings series g_iso_O-ring 23.6x1.8-B-ISO 3601-1', '', ( #17018 ) ) ;
#8096 = CARTESIAN_POINT ( 'NONE',  ( 29.14753769709988518, -3.271205139184214072, -3.627061608673662008 ) ) ;
#8097 = CARTESIAN_POINT ( 'NONE',  ( -2.038300084272748336E-14, -4.618802153517010289, -0.5000000000000000000 ) ) ;
#8098 = VECTOR ( 'NONE', #6006, 1000.000000000000000 ) ;
#8099 = CARTESIAN_POINT ( 'NONE',  ( 26.06734695949040059, -6.350061944625998933, -3.283357778048667797 ) ) ;
#8100 = DIRECTION ( 'NONE',  ( 0.000000000000000000, -1.000000000000000000, 0.000000000000000000 ) ) ;
#8101 = DIRECTION ( 'NONE',  ( 0.000000000000000000, 0.000000000000000000, -1.000000000000000000 ) ) ;
#8102 = CARTESIAN_POINT ( 'NONE',  ( 25.78518620311324838, -3.676302093007511651, -7.939653947423660263 ) ) ;
#8103 = CARTESIAN_POINT ( 'NONE',  ( 29.20951391065003122, -17.04067956308641030, -13.38411038749911697 ) ) ;
#8104 = ORIENTED_EDGE ( 'NONE', *, *, #11460, .F. ) ;
#8105 = CIRCLE ( 'NONE', #2036, 11.29999999999999893 ) ;
#8106 = EDGE_CURVE ( 'NONE', #5157, #8560, #16481, .T. ) ;
#8107 = AXIS2_PLACEMENT_3D ( 'NONE', #14183, #17009, #14373 ) ;
#8108 = CARTESIAN_POINT ( 'NONE',  ( 30.92509028327567933, -4.310986222078405206, 3.627061608673664228 ) ) ;
#8109 = CARTESIAN_POINT ( 'NONE',  ( 39.42387297280458114, -7.503110141889759888, -6.033357778048665132 ) ) ;
#8110 = CARTESIAN_POINT ( 'NONE',  ( 17.07932405232147488, -18.26192153598439205, 15.98801167710370663 ) ) ;
#8111 = ORIENTED_EDGE ( 'NONE', *, *, #9068, .T. ) ;
#8112 = CARTESIAN_POINT ( 'NONE',  ( 23.00000000000000000, -16.21813761408365195, 0.000000000000000000 ) ) ;
#8113 = VERTEX_POINT ( 'NONE', #17792 ) ;
#8114 = PLANE ( 'NONE',  #217 ) ;
#8115 = VERTEX_POINT ( 'NONE', #4052 ) ;
#8116 = LINE ( 'NONE', #6665, #7032 ) ;
#8118 = EDGE_CURVE ( 'NONE', #2263, #16382, #15810, .T. ) ;
#8117 = VECTOR ( 'NONE', #1131, 1000.000000000000227 ) ;
#8119 = CARTESIAN_POINT ( 'NONE',  ( 30.41294626588012306, -6.253601060580800564, -6.861505862736167138 ) ) ;
#8120 = DIRECTION ( 'NONE',  ( -0.5661261679878573094, 0.8243186046180107640, 0.000000000000000000 ) ) ;
#8121 = CARTESIAN_POINT ( 'NONE',  ( 28.19013153391124860, -7.158573733970061248, 5.783357778048669573 ) ) ;
#8122 = CARTESIAN_POINT ( 'NONE',  ( 25.95642634701329499, -4.403549397486667516, 7.880302681851837576 ) ) ;
#8123 = CARTESIAN_POINT ( 'NONE',  ( 28.88938074516742205, -6.437160617781993999, 6.861505862736158257 ) ) ;
#8124 = AXIS2_PLACEMENT_3D ( 'NONE', #6180, #830, #3289 ) ;
#8125 = DIRECTION ( 'NONE',  ( 0.3830490080632377725, -0.9237280213470682178, 0.000000000000000000 ) ) ;
#8126 = CARTESIAN_POINT ( 'NONE',  ( 28.16197717867739314, -7.161965777771100328, -5.113484796970856117 ) ) ;
#8127 = FACE_OUTER_BOUND ( 'NONE', #892, .T. ) ;
#8128 = ORIENTED_EDGE ( 'NONE', *, *, #15704, .T. ) ;
#8129 = CARTESIAN_POINT ( 'NONE',  ( 28.67914455963771303, -4.581578327848842669, 3.283357778048664244 ) ) ;
#8130 = ADVANCED_FACE ( 'NONE', ( #6774 ), #15114, .F. ) ;
#8131 = AXIS2_PLACEMENT_3D ( 'NONE', #11509, #17817, #2466 ) ;
#8132 = EDGE_LOOP ( 'NONE', ( #12165, #8733 ) ) ;
#8133 = EDGE_CURVE ( 'NONE', #8657, #8474, #6859, .T. ) ;
#8134 = AXIS2_PLACEMENT_3D ( 'NONE', #13690, #12238, #17810 ) ;
#8135 = ORIENTED_EDGE ( 'NONE', *, *, #12646, .T. ) ;
#8136 = ORIENTED_EDGE ( 'NONE', *, *, #14036, .T. ) ;
#8137 = CARTESIAN_POINT ( 'NONE',  ( 30.04066231269008469, -3.163601260824890904, 3.627061608673666893 ) ) ;
#8138 = CARTESIAN_POINT ( 'NONE',  ( 26.87785582392756112, -3.344784462964796035, 8.283357778048666020 ) ) ;
#8139 = ORIENTED_EDGE ( 'NONE', *, *, #6900, .T. ) ;
#8140 = CARTESIAN_POINT ( 'NONE',  ( 29.15206445563513071, -6.405512418264540209, 4.705209693361159573 ) ) ;
#8141 = CARTESIAN_POINT ( 'NONE',  ( 0.000000000000000000, 0.000000000000000000, -4.000000000000000000 ) ) ;
#8142 = CIRCLE ( 'NONE', #7851, 2.749999999999991118 ) ;
#8143 = CARTESIAN_POINT ( 'NONE',  ( -3.199999999999999289, 4.408728476930471151E-16, 2.399999999999999467 ) ) ;
#8144 = CARTESIAN_POINT ( 'NONE',  ( -1.917618200156724081E-28, -7.000000000000001776, 0.000000000000000000 ) ) ;
#8145 = DIRECTION ( 'NONE',  ( 0.000000000000000000, 0.000000000000000000, -1.000000000000000000 ) ) ;
#8146 = CARTESIAN_POINT ( 'NONE',  ( 26.24443550082169807, -6.794058631016747896, -7.409555870055547722 ) ) ;
#8147 = CARTESIAN_POINT ( 'NONE',  ( 28.72797218747911074, -6.756415940301135237, -4.533357778048668685 ) ) ;
#8148 = CARTESIAN_POINT ( 'NONE',  ( 25.76366024945007638, -10.60870341083598056, -14.29366788170017699 ) ) ;
#8149 = VECTOR ( 'NONE', #16966, 1000.000000000000114 ) ;
#8150 = CARTESIAN_POINT ( 'NONE',  ( 25.57853536445108489, -10.52124088318384310, 14.33864855032055985 ) ) ;
#8151 = ORIENTED_EDGE ( 'NONE', *, *, #1871, .F. ) ;
#8152 = AXIS2_PLACEMENT_3D ( 'NONE', #8177, #10953, #13709 ) ;
#8153 = CARTESIAN_POINT ( 'NONE',  ( 30.93831368681553684, -6.190304661545915188, -4.705209693361169343 ) ) ;
#8154 = CARTESIAN_POINT ( 'NONE',  ( 28.93739072872572393, -3.296523698798161650, -7.939653947423660263 ) ) ;
#8155 = AXIS2_PLACEMENT_3D ( 'NONE', #13025, #7336, #9932 ) ;
#8156 = FACE_OUTER_BOUND ( 'NONE', #1773, .T. ) ;
#8157 = CONICAL_SURFACE ( 'NONE', #3223, 3.999999999999998224, 0.8911886515913775009 ) ;
#8158 = CARTESIAN_POINT ( 'NONE',  ( 31.75254397038802878, -4.211294393702175398, -8.283357778048662468 ) ) ;
#8159 = EDGE_CURVE ( 'NONE', #2513, #10545, #17701, .T. ) ;
#8160 = EDGE_CURVE ( 'NONE', #9636, #14428, #15712, .T. ) ;
#8161 = EDGE_LOOP ( 'NONE', ( #4776, #17720, #9877, #2121 ) ) ;
#8162 = CARTESIAN_POINT ( 'NONE',  ( 32.65880277236253448, -4.102108105263264193, 3.627061608673664228 ) ) ;
#8163 = CIRCLE ( 'NONE', #354, 5.500000000000000888 ) ;
#8164 = CARTESIAN_POINT ( 'NONE',  ( 27.61527553138257574, -4.709753535998224550, -7.939653947423662039 ) ) ;
#8165 = CARTESIAN_POINT ( 'NONE',  ( -13.60000000000000320, 0.000000000000000000, 0.000000000000000000 ) ) ;
#8166 = CARTESIAN_POINT ( 'NONE',  ( -35.62429925076629189, -17.76690233603958902, 0.5379818257722508434 ) ) ;
#8167 = CARTESIAN_POINT ( 'NONE',  ( 30.01874226414561875, -2.539271660970221944, -6.861505862736159145 ) ) ;
#8168 = FACE_OUTER_BOUND ( 'NONE', #13558, .T. ) ;
#8169 = ADVANCED_FACE ( 'NONE', ( #17031 ), #15753, .F. ) ;
#8170 = DIRECTION ( 'NONE',  ( 0.9928203230275511881, 0.1196152422706614760, 0.000000000000000000 ) ) ;
#8171 = AXIS2_PLACEMENT_3D ( 'NONE', #11493, #8803, #11305 ) ;
#8172 = DIRECTION ( 'NONE',  ( 0.000000000000000000, -0.000000000000000000, 1.000000000000000000 ) ) ;
#8173 = CARTESIAN_POINT ( 'NONE',  ( 29.74110826630370497, -2.999819088432076786, -8.283357778048658915 ) ) ;
#8174 = ORIENTED_EDGE ( 'NONE', *, *, #7413, .T. ) ;
#8175 = DIRECTION ( 'NONE',  ( -0.000000000000000000, -0.000000000000000000, -1.000000000000000000 ) ) ;
#8176 = AXIS2_PLACEMENT_3D ( 'NONE', #8394, #1071, #14939 ) ;
#8177 = CARTESIAN_POINT ( 'NONE',  ( 0.000000000000000000, 0.000000000000000000, -12.00000000000000000 ) ) ;
#8178 = CYLINDRICAL_SURFACE ( 'NONE', #16156, 2.499999999999999112 ) ;
#8179 = CARTESIAN_POINT ( 'NONE',  ( 7.499998387031003411, -20.49508120620799900, 6.000000000000000000 ) ) ;
#8180 = CARTESIAN_POINT ( 'NONE',  ( -3.472352378023116692, -2.614038573344128924, -3.020318136128631981 ) ) ;
#8181 = CARTESIAN_POINT ( 'NONE',  ( 30.25080928106424594, -3.138282701210941994, -3.627061608673662896 ) ) ;
#8182 = CONICAL_SURFACE ( 'NONE', #950, 3.999999999999998224, 0.8911886515913775009 ) ;
#8183 = VECTOR ( 'NONE', #3049, 1000.000000000000000 ) ;
#8184 = VECTOR ( 'NONE', #16175, 1000.000000000000000 ) ;
#8185 = ADVANCED_FACE ( 'NONE', ( #11465 ), #4585, .T. ) ;
#8186 = CARTESIAN_POINT ( 'NONE',  ( 32.58190297908952004, -5.565186596593329149, -8.283357778048664244 ) ) ;
#8187 = ORIENTED_EDGE ( 'NONE', *, *, #3866, .F. ) ;
#8188 = CARTESIAN_POINT ( 'NONE',  ( 0.000000000000000000, 0.000000000000000000, 0.000000000000000000 ) ) ;
#8189 = VECTOR ( 'NONE', #13205, 1000.000000000000000 ) ;
#8190 = VERTEX_POINT ( 'NONE', #3143 ) ;
#8191 =( REPRESENTATION_RELATIONSHIP ('NONE','NONE', #3227, #12009 ) REPRESENTATION_RELATIONSHIP_WITH_TRANSFORMATION ( #3315 )SHAPE_REPRESENTATION_RELATIONSHIP( ) );
#8192 = EDGE_CURVE ( 'NONE', #12819, #16631, #6153, .T. ) ;
#8193 = CARTESIAN_POINT ( 'NONE',  ( 29.02054416436834217, -2.659534819136519790, -4.705209693361160461 ) ) ;
#8194 = FACE_BOUND ( 'NONE', #9415, .T. ) ;
#8195 = CARTESIAN_POINT ( 'NONE',  ( 33.27602027394517847, -2.146833986953896822, -4.705209693361161349 ) ) ;
#8196 = CARTESIAN_POINT ( 'NONE',  ( 45.50000000000000000, -16.03270077640482683, -2.787981825772258837 ) ) ;
#8197 = FACE_OUTER_BOUND ( 'NONE', #6426, .T. ) ;
#8198 = CARTESIAN_POINT ( 'NONE',  ( 25.96860978910007844, -6.167287525404733017, -7.540302725459484989 ) ) ;
#8199 = ORIENTED_EDGE ( 'NONE', *, *, #14396, .T. ) ;
#8200 = CARTESIAN_POINT ( 'NONE',  ( 18.06124445020232727, -20.07065898529088344, -15.83842874644866505 ) ) ;
#8201 = AXIS2_PLACEMENT_3D ( 'NONE', #2714, #17803, #13681 ) ;
#8202 = CARTESIAN_POINT ( 'NONE',  ( 30.40841950734487753, -3.119293781500474427, 7.939653947423664704 ) ) ;
#8203 = CARTESIAN_POINT ( 'NONE',  ( 38.92318875345451090, -3.347373306402334769, -5.783357778048662468 ) ) ;
#8204 = CARTESIAN_POINT ( 'NONE',  ( -4.207491450040567571, 2.029819825146473189, -3.371670828759567140 ) ) ;
#8205 = VERTEX_POINT ( 'NONE', #2967 ) ;
#8206 = CARTESIAN_POINT ( 'NONE',  ( 32.63137222500256485, -6.623491938275930302, -6.453230759126470595 ) ) ;
#8207 = ORIENTED_EDGE ( 'NONE', *, *, #13177, .F. ) ;
#8208 = CARTESIAN_POINT ( 'NONE',  ( 8.809730593168891843, -18.96833375928839516, 16.83727734034771473 ) ) ;
#8209 = ORIENTED_EDGE ( 'NONE', *, *, #1381, .F. ) ;
#8210 = CARTESIAN_POINT ( 'NONE',  ( 33.95908713831673964, -3.945449517755637014, -5.783357778048663356 ) ) ;
#8211 = CARTESIAN_POINT ( 'NONE',  ( 30.40841950734487753, -3.119293781500474427, -3.627061608673662008 ) ) ;
#8212 = ADVANCED_FACE ( 'NONE', ( #14202 ), #9898, .T. ) ;
#8213 = CARTESIAN_POINT ( 'NONE',  ( 25.11802603177690330, -16.03270077640482683, -0.5379818257722508434 ) ) ;
#8214 = CARTESIAN_POINT ( 'NONE',  ( 31.05948030073166066, -1.776715885202022394, -5.783357778048661579 ) ) ;
#8215 = DIRECTION ( 'NONE',  ( 0.000000000000000000, 0.000000000000000000, 1.000000000000000000 ) ) ;
#8216 = CARTESIAN_POINT ( 'NONE',  ( 32.77701044293393551, -4.087866415376695706, 8.283357778048662468 ) ) ;
#8217 = CARTESIAN_POINT ( 'NONE',  ( 27.61527553138257574, -4.709753535998224550, 3.627061608673664228 ) ) ;
#8218 = PLANE ( 'NONE',  #2399 ) ;
#8219 = LINE ( 'NONE', #14021, #4295 ) ;
#8220 = LINE ( 'NONE', #2600, #14533 ) ;
#8221 = VERTEX_POINT ( 'NONE', #8492 ) ;
#8222 = EDGE_LOOP ( 'NONE', ( #10404, #5733, #10372, #6973 ) ) ;
#8223 = CARTESIAN_POINT ( 'NONE',  ( 32.77257290155422709, -2.834459985843461816, 7.939653947423664704 ) ) ;
#8224 = CARTESIAN_POINT ( 'NONE',  ( 26.64639396487419987, -2.308405637095112706, 5.783357778048667797 ) ) ;
#8225 = EDGE_LOOP ( 'NONE', ( #8739, #4884, #17427, #11989, #15859 ) ) ;
#8226 = CARTESIAN_POINT ( 'NONE',  ( 29.52399153675929355, -1.971908820246954130, 5.783357778048668685 ) ) ;
#8227 = CARTESIAN_POINT ( 'NONE',  ( -5.781152949374509298, 1.605699403978974260, -1.901951201008075243 ) ) ;
#8228 = CARTESIAN_POINT ( 'NONE',  ( 0.000000000000000000, 0.000000000000000000, -12.00000000000000000 ) ) ;
#8229 = CARTESIAN_POINT ( 'NONE',  ( 0.000000000000000000, 0.000000000000000000, 0.000000000000000000 ) ) ;
#8230 = DIRECTION ( 'NONE',  ( -1.000000000000000000, 0.000000000000000000, -0.000000000000000000 ) ) ;
#8231 = CARTESIAN_POINT ( 'NONE',  ( -25.11802603177690330, -19.03270077640482683, -10.53798182577225084 ) ) ;
#8232 = CARTESIAN_POINT ( 'NONE',  ( 29.81991338116587542, -2.990324628369393611, -8.283357778048658915 ) ) ;
#8233 = CARTESIAN_POINT ( 'NONE',  ( 26.01652455409633902, -4.902371455920926380, 5.783357778048663356 ) ) ;
#8234 = EDGE_CURVE ( 'NONE', #11271, #1184, #7232, .T. ) ;
#8235 = B_SPLINE_CURVE_WITH_KNOTS ( 'NONE', 3,
 ( #17635, #819, #7897, #6349 ),
 .UNSPECIFIED., .F., .F.,
 ( 4, 4 ),
 ( 2.843119637691541009E-07, 0.001422633878257847928 ),
 .UNSPECIFIED. ) ;
#8236 = CARTESIAN_POINT ( 'NONE',  ( 0.6937372685066659495, -4.453844082567731455, -3.310536846335892847 ) ) ;
#8237 = DIRECTION ( 'NONE',  ( 0.8660254037844328234, -0.5000000000000099920, 0.000000000000000000 ) ) ;
#8238 =( NAMED_UNIT ( * ) SI_UNIT ( $, .STERADIAN. ) SOLID_ANGLE_UNIT ( ) );
#8239 = CARTESIAN_POINT ( 'NONE',  ( 29.15206445563513071, -6.405512418264540209, -6.861505862736167138 ) ) ;
#8240 = CARTESIAN_POINT ( 'NONE',  ( 30.29464937815318493, -4.386941900920275472, -7.939653947423662039 ) ) ;
#8241 = ORIENTED_EDGE ( 'NONE', *, *, #1824, .F. ) ;
#8242 = CARTESIAN_POINT ( 'NONE',  ( 26.07857582428556853, -4.894895503279006022, 3.283357778048664244 ) ) ;
#8243 = CARTESIAN_POINT ( 'NONE',  ( -7.499998387031003411, -20.49508120620799900, -6.000000000000000000 ) ) ;
#8244 = ORIENTED_EDGE ( 'NONE', *, *, #5099, .F. ) ;
#8245 = PRODUCT ( 'ceramic piston', 'ceramic piston', '', ( #5835 ) ) ;
#8246 = ORIENTED_EDGE ( 'NONE', *, *, #6483, .F. ) ;
#8247 = CARTESIAN_POINT ( 'NONE',  ( 33.42946061375642586, -6.517141185936593750, 5.783357778048658915 ) ) ;
#8248 = CARTESIAN_POINT ( 'NONE',  ( 27.93049598394382116, -4.671775696577297410, -3.627061608673664672 ) ) ;
#8249 = CARTESIAN_POINT ( 'NONE',  ( 8.632250723006720250, -18.84644399697197770, -13.00000000000000178 ) ) ;
#8250 = FACE_OUTER_BOUND ( 'NONE', #11588, .T. ) ;
#8251 = CARTESIAN_POINT ( 'NONE',  ( 28.34209327568754233, -5.876127416962207306, -7.939653947423664704 ) ) ;
#8252 = CARTESIAN_POINT ( 'NONE',  ( 32.29220775574281532, -1.628196571319322050, 5.113484796970859669 ) ) ;
#8253 = CARTESIAN_POINT ( 'NONE',  ( 41.90164972253718645, -2.988527579590353422, -5.783357778048662468 ) ) ;
#8254 = CARTESIAN_POINT ( 'NONE',  ( 0.000000000000000000, 0.000000000000000000, -10.00000000000000000 ) ) ;
#8255 = EDGE_CURVE ( 'NONE', #15783, #7031, #1242, .T. ) ;
#8256 = CARTESIAN_POINT ( 'NONE',  ( 27.15176839919044482, -1.857969822100365098, -5.783357778048658027 ) ) ;
#8257 = ORIENTED_EDGE ( 'NONE', *, *, #16240, .F. ) ;
#8258 = CARTESIAN_POINT ( 'NONE',  ( 4.000000000000000000, 2.309401076758498483, -3.133295621305380863 ) ) ;
#8259 = DIRECTION ( 'NONE',  ( 0.9928203230275510771, 0.1196152422706609902, 4.006172263299092517E-17 ) ) ;
#8260 = DIRECTION ( 'NONE',  ( 0.8191520442889900222, 1.003171929053522528E-16, -0.5735764363510486019 ) ) ;
#8261 = CARTESIAN_POINT ( 'NONE',  ( 0.000000000000000000, 0.000000000000000000, -3.000000000000002665 ) ) ;
#8262 = CARTESIAN_POINT ( 'NONE',  ( 10.50000000000000000, 1.285879139104720831E-15, -4.000000000000000000 ) ) ;
#8263 = CARTESIAN_POINT ( 'NONE',  ( 30.25533603959949502, -6.272589980291270351, -6.861505862736166250 ) ) ;
#8264 = EDGE_LOOP ( 'NONE', ( #7122, #6879, #11445, #14602 ) ) ;
#8265 = ORIENTED_EDGE ( 'NONE', *, *, #8718, .F. ) ;
#8266 = LINE ( 'NONE', #4194, #6218 ) ;
#8267 = DIRECTION ( 'NONE',  ( 1.000000000000000000, 0.000000000000000000, 0.000000000000000000 ) ) ;
#8268 = CARTESIAN_POINT ( 'NONE',  ( -29.25000000000000000, -16.21813761408365195, -13.37255996287876947 ) ) ;
#8269 = VERTEX_POINT ( 'NONE', #7144 ) ;
#8270 = CARTESIAN_POINT ( 'NONE',  ( 30.17635249042624679, -2.520282741259753045, -6.861505862736158257 ) ) ;
#8271 = LINE ( 'NONE', #17159, #16550 ) ;
#8272 = EDGE_CURVE ( 'NONE', #11446, #9144, #13744, .T. ) ;
#8273 = CARTESIAN_POINT ( 'NONE',  ( 32.54503264317084188, -5.369756224683081669, -3.627061608673667781 ) ) ;
#8274 = DIRECTION ( 'NONE',  ( 0.000000000000000000, 0.000000000000000000, 1.000000000000000000 ) ) ;
#8275 = DIRECTION ( 'NONE',  ( 0.000000000000000000, 0.000000000000000000, -1.000000000000000000 ) ) ;
#8276 = CARTESIAN_POINT ( 'NONE',  ( 27.77288575766320378, -4.690764616287755651, -7.939653947423662039 ) ) ;
#8277 = CARTESIAN_POINT ( 'NONE',  ( 29.34405387406022570, -7.019548880150045633, 6.453230759126462601 ) ) ;
#8278 = ADVANCED_FACE ( 'NONE', ( #5850 ), #1834, .T. ) ;
#8279 =( BOUNDED_CURVE ( )  B_SPLINE_CURVE ( 2, ( #12907, #10081, #12634, #4213, #9714, #11244, #2843, #15358, #2938 ),
 .UNSPECIFIED., .F., .T. ) 
 B_SPLINE_CURVE_WITH_KNOTS ( ( 3, 2, 2, 2, 3 ),
 ( 0.01923076923076925265, 0.02564102564102564014, 0.03846153846153846367, 0.05128205128205128027, 0.05769230769230771633 ),
 .UNSPECIFIED. ) 
 CURVE ( )  GEOMETRIC_REPRESENTATION_ITEM ( )  RATIONAL_B_SPLINE_CURVE ( ( 0.9330127018922194093, 0.9330127018922196314, 1.000000000000000000, 0.8660254037844387076, 1.000000000000000000, 0.8660254037844387076, 1.000000000000000000, 0.9330127018922190762, 0.9330127018922194093 ) ) 
 REPRESENTATION_ITEM ( '' )  );
#8280 =( BOUNDED_CURVE ( )  B_SPLINE_CURVE ( 2, ( #22, #16524, #9783, #3017, #7102, #12526, #13986, #8352, #16800 ),
 .UNSPECIFIED., .F., .T. ) 
 B_SPLINE_CURVE_WITH_KNOTS ( ( 3, 2, 2, 2, 3 ),
 ( 0.4423076923076923461, 0.4487179487179487336, 0.4615384615384615641, 0.4743589743589743390, 0.4807692307692307820 ),
 .UNSPECIFIED. ) 
 CURVE ( )  GEOMETRIC_REPRESENTATION_ITEM ( )  RATIONAL_B_SPLINE_CURVE ( ( 0.9330127018922194093, 0.9330127018922196314, 1.000000000000000000, 0.8660254037844387076, 1.000000000000000000, 0.8660254037844387076, 1.000000000000000000, 0.9330127018922190762, 0.9330127018922194093 ) ) 
 REPRESENTATION_ITEM ( '' )  );
#8281 = CARTESIAN_POINT ( 'NONE',  ( 27.12922144900085186, -2.887401855662130146, 6.861505862736166250 ) ) ;
#8282 = CARTESIAN_POINT ( 'NONE',  ( -5.781152949374509298, 1.605699403978974260, -3.000000000000000888 ) ) ;
#8283 = DIRECTION ( 'NONE',  ( -0.7403740928408700794, 0.6721950629468047556, -3.769102058307143718E-16 ) ) ;
#8284 = VERTEX_POINT ( 'NONE', #12745 ) ;
#8285 = DIRECTION ( 'NONE',  ( -1.000000000000000000, 0.000000000000000000, 0.000000000000000000 ) ) ;
#8286 = VERTEX_POINT ( 'NONE', #343 ) ;
#8287 = FACE_OUTER_BOUND ( 'NONE', #10153, .T. ) ;
#8288 = ORIENTED_EDGE ( 'NONE', *, *, #14300, .F. ) ;
#8289 = DIRECTION ( 'NONE',  ( -0.1196152422706610735, 0.9928203230275511881, 0.000000000000000000 ) ) ;
#8290 = CARTESIAN_POINT ( 'NONE',  ( 31.03886041246737548, -3.043338102658604161, -3.627061608673662008 ) ) ;
#8292 = ADVANCED_FACE ( 'NONE', ( #4499 ), #7041, .T. ) ;
#8291 = UNCERTAINTY_MEASURE_WITH_UNIT (LENGTH_MEASURE( 1.000000000000000082E-05 ), #9216, 'distance_accuracy_value', 'NONE');
#8293 = CARTESIAN_POINT ( 'NONE',  ( 30.45035428628836627, -2.914368949527523789, -8.283357778048660691 ) ) ;
#8294 = CARTESIAN_POINT ( 'NONE',  ( 27.99987602667382802, -2.482696394238434578, -4.533357778048659803 ) ) ;
#8295 = DIRECTION ( 'NONE',  ( 0.000000000000000000, 0.000000000000000000, 1.000000000000000000 ) ) ;
#8296 = CARTESIAN_POINT ( 'NONE',  ( 30.37838863598085837, -1.858773980305536089, -5.113484796970855228 ) ) ;
#8297 = CARTESIAN_POINT ( 'NONE',  ( 29.39282811755836633, -5.749534618892433002, 7.939653947423658487 ) ) ;
#8298 = LINE ( 'NONE', #13827, #6723 ) ;
#8299 = FACE_OUTER_BOUND ( 'NONE', #16743, .T. ) ;
#8300 = ADVANCED_FACE ( 'NONE', ( #16748 ), #10014, .F. ) ;
#8301 = FACE_OUTER_BOUND ( 'NONE', #3541, .T. ) ;
#8302 = ORIENTED_EDGE ( 'NONE', *, *, #4069, .T. ) ;
#8303 = EDGE_LOOP ( 'NONE', ( #10942, #16420, #11233, #11376 ) ) ;
#8304 = ADVANCED_FACE ( 'NONE', ( #5940 ), #12569, .T. ) ;
#8305 = CARTESIAN_POINT ( 'NONE',  ( 27.10313151398701947, -6.652368374500619908, 4.705209693361160461 ) ) ;
#8306 = DIRECTION ( 'NONE',  ( -0.05980762113533058533, 0.4964101615137755386, 0.8660254037844385966 ) ) ;
#8307 = ORIENTED_EDGE ( 'NONE', *, *, #10304, .T. ) ;
#8308 = CARTESIAN_POINT ( 'NONE',  ( 27.89118264539014547, -6.557423775948280742, 4.705209693361159573 ) ) ;
#8309 = CARTESIAN_POINT ( 'NONE',  ( -38.15522249139979749, -7.597641695372263193, 5.783357778048663356 ) ) ;
#8310 = DIRECTION ( 'NONE',  ( -1.000000000000000000, 0.000000000000000000, 0.000000000000000000 ) ) ;
#8311 = DIRECTION ( 'NONE',  ( 0.000000000000000000, 0.000000000000000000, 1.000000000000000000 ) ) ;
#8312 = CARTESIAN_POINT ( 'NONE',  ( 27.28266178881210280, -7.257709054644824853, -5.783357778048669573 ) ) ;
#8313 = DIRECTION ( 'NONE',  ( 0.9928203230275510771, 0.1196152422706609902, 4.006172263299092517E-17 ) ) ;
#8314 = CARTESIAN_POINT ( 'NONE',  ( 31.24973580796908834, -6.452593224933654170, -4.533357778048668685 ) ) ;
#8315 = FACE_OUTER_BOUND ( 'NONE', #896, .T. ) ;
#8316 = CIRCLE ( 'NONE', #7185, 6.000000000000000888 ) ;
#8317 = EDGE_CURVE ( 'NONE', #3497, #15348, #7025, .T. ) ;
#8318 = CARTESIAN_POINT ( 'NONE',  ( 25.57853536445108489, -10.52124088318384310, -14.33864855032055985 ) ) ;
#8319 = CARTESIAN_POINT ( 'NONE',  ( 26.01595305975170547, -2.384361315936983416, 5.783357778048657138 ) ) ;
#8320 = CARTESIAN_POINT ( 'NONE',  ( 29.17398450417959310, -7.029842018119214941, -5.783357778048669573 ) ) ;
#8321 = CARTESIAN_POINT ( 'NONE',  ( 28.40332666278570173, -4.614808937445885384, -7.939653947423662039 ) ) ;
#8322 = DIRECTION ( 'NONE',  ( 0.000000000000000000, 0.000000000000000000, 1.000000000000000000 ) ) ;
#8323 = DIRECTION ( 'NONE',  ( -0.9928203230275512992, -0.1196152422706610319, -9.614813431917826478E-17 ) ) ;
#8324 = EDGE_LOOP ( 'NONE', ( #3941, #5942 ) ) ;
#8325 = ORIENTED_EDGE ( 'NONE', *, *, #2157, .T. ) ;
#8326 = EDGE_CURVE ( 'NONE', #12636, #13340, #11656, .T. ) ;
#8327 = CARTESIAN_POINT ( 'NONE',  ( 32.77709966008947617, -5.968767264923789284, 4.705209693361160461 ) ) ;
#8328 = DIRECTION ( 'NONE',  ( 0.9928203230275511881, 0.1196152422706610735, 9.614813431917827710E-17 ) ) ;
#8329 = FACE_OUTER_BOUND ( 'NONE', #1818, .T. ) ;
#8330 = CARTESIAN_POINT ( 'NONE',  ( 32.50309786422735669, -5.574681056656013212, -8.283357778048664244 ) ) ;
#8331 = DIRECTION ( 'NONE',  ( -1.224646799147353207E-16, 1.000000000000000000, 0.000000000000000000 ) ) ;
#8332 = CARTESIAN_POINT ( 'NONE',  ( 30.90769699326644826, -6.820963901304073929, -5.783357778048668685 ) ) ;
#8333 = CARTESIAN_POINT ( 'NONE',  ( 32.63137222500256485, -6.623491938275930302, 5.113484796970852564 ) ) ;
#8334 = DIRECTION ( 'NONE',  ( 0.000000000000000000, 0.000000000000000000, 1.000000000000000000 ) ) ;
#8335 = B_SPLINE_CURVE_WITH_KNOTS ( 'NONE', 3,
 ( #13124, #4947, #6135, #787, #9041 ),
 .UNSPECIFIED., .F., .F.,
 ( 4, 1, 4 ),
 ( 0.000000000000000000, 0.002309401076758505356, 0.004618802153517009845 ),
 .UNSPECIFIED. ) ;
#8336 = VECTOR ( 'NONE', #10322, 1000.000000000000227 ) ;
#8337 = CARTESIAN_POINT ( 'NONE',  ( 26.82912971812490355, -6.258282166232842947, -8.283357778048662468 ) ) ;
#8338 = VECTOR ( 'NONE', #2312, 1000.000000000000000 ) ;
#8339 = VERTEX_POINT ( 'NONE', #781 ) ;
#8340 = CARTESIAN_POINT ( 'NONE',  ( 30.90769699326644826, -6.820963901304073929, -5.783357778048668685 ) ) ;
#8341 = AXIS2_PLACEMENT_3D ( 'NONE', #7935, #7752, #2330 ) ;
#8342 = CARTESIAN_POINT ( 'NONE',  ( 27.87912141988533676, -2.159886323212414361, -6.453230759126469707 ) ) ;
#8343 = FACE_BOUND ( 'NONE', #14179, .T. ) ;
#8344 = B_SPLINE_CURVE_WITH_KNOTS ( 'NONE', 3,
 ( #697, #16033, #8856, #17312, #2246, #1975 ),
 .UNSPECIFIED., .F., .F.,
 ( 4, 2, 4 ),
 ( 0.002365888236227995951, 0.003551327329835086283, 0.004736766423442176181 ),
 .UNSPECIFIED. ) ;
#8345 = CARTESIAN_POINT ( 'NONE',  ( 34.23532670761333918, -6.238269840783189579, -1.783357778048662690 ) ) ;
#8346 = CARTESIAN_POINT ( 'NONE',  ( 30.80688261270428541, -4.325227911964988792, -3.283357778048664688 ) ) ;
#8347 = CARTESIAN_POINT ( 'NONE',  ( 31.27600417729400917, -6.449428405189353342, 4.533357778048659803 ) ) ;
#8348 = CARTESIAN_POINT ( 'NONE',  ( 30.02326902268086428, -5.673578940050561847, -3.627061608673667781 ) ) ;
#8349 = ORIENTED_EDGE ( 'NONE', *, *, #10304, .F. ) ;
#8350 = EDGE_CURVE ( 'NONE', #475, #3798, #5858, .T. ) ;
#8351 = DIRECTION ( 'NONE',  ( 0.9928203230275510771, 0.1196152422706614621, -0.000000000000000000 ) ) ;
#8352 = CARTESIAN_POINT ( 'NONE',  ( 29.74794773085836397, -1.934729659147405689, -5.113484796970855228 ) ) ;
#8353 = CIRCLE ( 'NONE', #8931, 12.50000000000000000 ) ;
#8354 = ORIENTED_EDGE ( 'NONE', *, *, #10602, .F. ) ;
#8355 = CARTESIAN_POINT ( 'NONE',  ( -16.79182286896198306, -15.38653328895459893, -16.02976683711036898 ) ) ;
#8356 = ORIENTED_EDGE ( 'NONE', *, *, #9412, .F. ) ;
#8357 = CARTESIAN_POINT ( 'NONE',  ( 29.54591158530375239, -2.596238420101622868, -6.861505862736158257 ) ) ;
#8358 = DIRECTION ( 'NONE',  ( -1.000000000000000000, 0.000000000000000000, 0.000000000000000000 ) ) ;
#8359 = VECTOR ( 'NONE', #7844, 1000.000000000000000 ) ;
#8360 = CARTESIAN_POINT ( 'NONE',  ( 28.98992747081925359, -3.290194058894681639, -3.627061608673662896 ) ) ;
#8361 = CARTESIAN_POINT ( 'NONE',  ( -2.016448651773435938E-27, -20.49999999999999645, 6.000000000000000000 ) ) ;
#8362 = CARTESIAN_POINT ( 'NONE',  ( 4.000000000000000000, 1.680235903636325023, -3.016633206402969503 ) ) ;
#8363 = CARTESIAN_POINT ( 'NONE',  ( 27.02867472334902033, -6.034368414549446058, -3.627061608673668225 ) ) ;
#8364 = VECTOR ( 'NONE', #3376, 1000.000000000000227 ) ;
#8365 = ORIENTED_EDGE ( 'NONE', *, *, #17857, .T. ) ;
#8366 = CARTESIAN_POINT ( 'NONE',  ( 20.84394630543432569, -22.08803114836474890, -15.35658910651175013 ) ) ;
#8367 = ORIENTED_EDGE ( 'NONE', *, *, #3653, .F. ) ;
#8368 = AXIS2_PLACEMENT_3D ( 'NONE', #9891, #11333, #7112 ) ;
#8369 = EDGE_CURVE ( 'NONE', #13928, #2781, #14390, .T. ) ;
#8370 = CARTESIAN_POINT ( 'NONE',  ( 27.77288575766320378, -4.690764616287755651, 3.627061608673664228 ) ) ;
#8371 = CARTESIAN_POINT ( 'NONE',  ( -25.76436512043297711, -21.83811057962065405, 14.29411090273705831 ) ) ;
#8372 = CARTESIAN_POINT ( 'NONE',  ( -37.55714628004649569, -12.56174331051002113, 5.783357778048663356 ) ) ;
#8373 = ORIENTED_EDGE ( 'NONE', *, *, #17630, .F. ) ;
#8374 = PLANE ( 'NONE',  #7898 ) ;
#8375 = VERTEX_POINT ( 'NONE', #15838 ) ;
#8376 = CARTESIAN_POINT ( 'NONE',  ( 20.00000000000000000, 7.999999999999996447, -15.51150668642334374 ) ) ;
#8377 = ORIENTED_EDGE ( 'NONE', *, *, #8075, .T. ) ;
#8378 = CARTESIAN_POINT ( 'NONE',  ( 33.69269431359690969, -6.158264969628857166, -4.533357778048668685 ) ) ;
#8379 = CARTESIAN_POINT ( 'NONE',  ( 26.19678349485696955, -4.880653813392439311, -3.627061608673664672 ) ) ;
#8380 = FACE_BOUND ( 'NONE', #5596, .T. ) ;
#8381 = CARTESIAN_POINT ( 'NONE',  ( 29.86122125502053848, -4.439161430227785310, 3.283357778048664244 ) ) ;
#8382 = APPLICATION_PROTOCOL_DEFINITION ( 'draft international standard', 'automotive_design', 1998, #4243 ) ;
#8383 = CARTESIAN_POINT ( 'NONE',  ( 33.40745134805642635, -4.011910736534825439, -3.283357778048664688 ) ) ;
#8384 = AXIS2_PLACEMENT_3D ( 'NONE', #2347, #978, #16215 ) ;
#8385 =( BOUNDED_CURVE ( )  B_SPLINE_CURVE ( 2, ( #6675, #9558, #10649, #5389, #7956, #5304, #8036, #16393, #12206 ),
 .UNSPECIFIED., .F., .F. ) 
 B_SPLINE_CURVE_WITH_KNOTS ( ( 3, 2, 2, 2, 3 ),
 ( 0.1730769230769231004, 0.1794871794871794879, 0.1923076923076923184, 0.2051282051282051211, 0.2115384615384615641 ),
 .UNSPECIFIED. ) 
 CURVE ( )  GEOMETRIC_REPRESENTATION_ITEM ( )  RATIONAL_B_SPLINE_CURVE ( ( 0.9330127018922194093, 0.9330127018922196314, 1.000000000000000000, 0.8660254037844387076, 1.000000000000000000, 0.8660254037844387076, 1.000000000000000000, 0.9330127018922190762, 0.9330127018922194093 ) ) 
 REPRESENTATION_ITEM ( '' )  );
#8386 = CARTESIAN_POINT ( 'NONE',  ( 28.36401332423200827, -6.500457016816879374, 4.705209693361160461 ) ) ;
#8387 = LINE ( 'NONE', #15467, #653 ) ;
#8388 = CARTESIAN_POINT ( 'NONE',  ( 28.91547068018125799, -2.672194098943493135, 4.705209693361168455 ) ) ;
#8389 = VECTOR ( 'NONE', #2341, 1000.000000000000114 ) ;
#8390 = ORIENTED_EDGE ( 'NONE', *, *, #17406, .F. ) ;
#8391 = EDGE_CURVE ( 'NONE', #3302, #4053, #4762, .T. ) ;
#8392 = ORIENTED_EDGE ( 'NONE', *, *, #9625, .T. ) ;
#8393 = CARTESIAN_POINT ( 'NONE',  ( 27.30005507882132676, -4.747731375419166788, 7.939653947423662039 ) ) ;
#8394 = CARTESIAN_POINT ( 'NONE',  ( 38.92318875345451090, -3.347373306402334769, -5.783357778048662468 ) ) ;
#8395 = AXIS2_PLACEMENT_3D ( 'NONE', #17765, #13730, #4122 ) ;
#8396 = ORIENTED_EDGE ( 'NONE', *, *, #14838, .T. ) ;
#8397 = CARTESIAN_POINT ( 'NONE',  ( 27.02414796481377124, -2.900061135469103490, 4.705209693361168455 ) ) ;
#8398 = CARTESIAN_POINT ( 'NONE',  ( 26.01652455409633902, -4.902371455920926380, 5.783357778048663356 ) ) ;
#8399 = DIRECTION ( 'NONE',  ( 0.000000000000000000, 0.000000000000000000, 1.000000000000000000 ) ) ;
#8400 = ORIENTED_EDGE ( 'NONE', *, *, #16124, .F. ) ;
#8401 = DIRECTION ( 'NONE',  ( 0.9928203230275510771, 0.1196152422706609902, 4.006172263299092517E-17 ) ) ;
#8402 = PLANE ( 'NONE',  #9619 ) ;
#8403 = DIRECTION ( 'NONE',  ( 0.9928203230275510771, 0.1196152422706614621, -0.000000000000000000 ) ) ;
#8404 = CARTESIAN_POINT ( 'NONE',  ( 26.31556265977298992, -7.384422263489805793, -5.783357778048663356 ) ) ;
#8405 = EDGE_CURVE ( 'NONE', #14045, #7467, #17193, .T. ) ;
#8406 = CARTESIAN_POINT ( 'NONE',  ( 30.88568772756644520, -4.315733451902305617, -3.283357778048664688 ) ) ;
#8407 = DIRECTION ( 'NONE',  ( -0.000000000000000000, 1.000000000000000000, -0.000000000000000000 ) ) ;
#8408 = CARTESIAN_POINT ( 'NONE',  ( 18.46842688268906230, -11.90892979872008084, -15.77307170257308933 ) ) ;
#8409 = FACE_OUTER_BOUND ( 'NONE', #6173, .T. ) ;
#8410 = CARTESIAN_POINT ( 'NONE',  ( 30.15026255541241440, -6.285249260098253465, -4.705209693361168455 ) ) ;
#8411 =( BOUNDED_CURVE ( )  B_SPLINE_CURVE ( 2, ( #5762, #15120, #17959, #16574, #12578 ),
 .UNSPECIFIED., .F., .T. ) 
 B_SPLINE_CURVE_WITH_KNOTS ( ( 3, 2, 3 ),
 ( 0.000000000000000000, 0.01282051282051282007, 0.01923076923076924918 ),
 .UNSPECIFIED. ) 
 CURVE ( )  GEOMETRIC_REPRESENTATION_ITEM ( )  RATIONAL_B_SPLINE_CURVE ( ( 1.000000000000000000, 0.8660254037844387076, 1.000000000000000000, 0.9330127018922191873, 0.9330127018922194093 ) ) 
 REPRESENTATION_ITEM ( '' )  );
#8412 = CARTESIAN_POINT ( 'NONE',  ( 29.17398450417959310, -7.029842018119214941, -5.783357778048669573 ) ) ;
#8413 = CONICAL_SURFACE ( 'NONE', #7266, 9.500000000000001776, 0.7853981633974465026 ) ;
#8414 = DIRECTION ( 'NONE',  ( 1.000000000000000000, 0.000000000000000000, 0.000000000000000000 ) ) ;
#8415 = ORIENTED_EDGE ( 'NONE', *, *, #17570, .T. ) ;
#8416 = EDGE_LOOP ( 'NONE', ( #9081, #9699, #2724, #6143 ) ) ;
#8417 = ORIENTED_EDGE ( 'NONE', *, *, #16179, .F. ) ;
#8418 = MECHANICAL_DESIGN_GEOMETRIC_PRESENTATION_REPRESENTATION (  '', ( #7852 ), #14803 ) ;
#8419 = CARTESIAN_POINT ( 'NONE',  ( 28.75786045390062995, -2.691183018653962034, 4.705209693361167567 ) ) ;
#8420 =( BOUNDED_SURFACE ( )  B_SPLINE_SURFACE ( 3, 2, ( 
 ( #13214, #15846, #13483 ),
 ( #12019, #6318, #4950 ),
 ( #6138, #10478, #2254 ),
 ( #13300, #5041, #10564 ),
 ( #12372, #15272, #10993 ),
 ( #1144, #2773, #13821 ) ),
 .UNSPECIFIED., .F., .F., .T. ) 
 B_SPLINE_SURFACE_WITH_KNOTS ( ( 4, 2, 4 ),
 ( 3, 3 ),
 ( 0.02023740217035200836, 0.02269762987400599646, 0.02515785757765998457 ),
 ( 0.000000000000000000, 1.000000000000000000 ),
 .UNSPECIFIED. ) 
 GEOMETRIC_REPRESENTATION_ITEM ( )  RATIONAL_B_SPLINE_SURFACE ( (
 ( 1.000000000000000000, 0.8047781539129729156, 1.000000000000000000),
 ( 1.000000000000000000, 0.8123770319056426992, 1.000000000000000000),
 ( 1.000000000000000000, 0.8190663783057815506, 1.000000000000000000),
 ( 1.000000000000000000, 0.8192359702876089722, 1.000000000000000000),
 ( 1.000000000000000000, 0.8126134888420550872, 1.000000000000000000),
 ( 1.000000000000000000, 0.8047712368238109093, 1.000000000000000000) ) ) 
 REPRESENTATION_ITEM ( '' )  SURFACE ( )  );
#8421 = CARTESIAN_POINT ( 'NONE',  ( 26.03917326857634151, -4.899642733102906433, -3.627061608673664672 ) ) ;
#8422 = DIRECTION ( 'NONE',  ( 0.1196152422706590474, -0.9928203230275514102, 0.000000000000000000 ) ) ;
#8423 = CARTESIAN_POINT ( 'NONE',  ( -4.914599809708808387, 17.56967244544484075, -17.00000000000000711 ) ) ;
#8424 = CARTESIAN_POINT ( 'NONE',  ( 0.000000000000000000, 0.000000000000000000, 8.700000000000001066 ) ) ;
#8425 = CARTESIAN_POINT ( 'NONE',  ( 30.25533603959949502, -6.272589980291270351, -6.861505862736166250 ) ) ;
#8426 = LINE ( 'NONE', #4525, #4087 ) ;
#8427 = FACE_BOUND ( 'NONE', #679, .T. ) ;
#8428 = AXIS2_PLACEMENT_3D ( 'NONE', #1089, #6613, #14956 ) ;
#8429 = CARTESIAN_POINT ( 'NONE',  ( 27.27683486999669427, -2.232449958253242883, -5.783357778048658027 ) ) ;
#8430 = CARTESIAN_POINT ( 'NONE',  ( 28.01872616749444944, -6.841866079205687790, -4.533357778048668685 ) ) ;
#8431 = AXIS2_PLACEMENT_3D ( 'NONE', #14881, #5519, #9592 ) ;
#8432 = ADVANCED_FACE ( 'NONE', ( #4940 ), #10288, .F. ) ;
#8433 = CARTESIAN_POINT ( 'NONE',  ( 30.25533603959949502, -6.272589980291270351, -6.861505862736166250 ) ) ;
#8434 = B_SPLINE_CURVE_WITH_KNOTS ( 'NONE', 3,
 ( #7221, #12731, #10092, #5834, #8661, #16735, #7313, #12832 ),
 .UNSPECIFIED., .F., .F.,
 ( 4, 2, 2, 4 ),
 ( 0.005725059856848623528, 0.006314084072593609265, 0.006903108288338595869, 0.008081156719828567342 ),
 .UNSPECIFIED. ) ;
#8435 = LINE ( 'NONE', #15156, #44 ) ;
#8436 = DIRECTION ( 'NONE',  ( 0.9928203230275510771, 0.1196152422706609902, 4.006172263299092517E-17 ) ) ;
#8437 = DIRECTION ( 'NONE',  ( -0.000000000000000000, -0.000000000000000000, -1.000000000000000000 ) ) ;
#8438 = B_SPLINE_CURVE_WITH_KNOTS ( 'NONE', 3,
 ( #15099, #16646, #3951, #12294, #5563, #16389 ),
 .UNSPECIFIED., .F., .F.,
 ( 4, 2, 4 ),
 ( 0.003358874760055536278, 0.004541967308452079903, 0.005725059856848623528 ),
 .UNSPECIFIED. ) ;
#8439 = CARTESIAN_POINT ( 'NONE',  ( 30.58169613980036772, -2.898544849976259385, -3.283357778048662023 ) ) ;
#8440 = CARTESIAN_POINT ( 'NONE',  ( 33.55383270609817714, -5.448088258586239796, 8.283357778048658915 ) ) ;
#8441 = CARTESIAN_POINT ( 'NONE',  ( 27.75549246765397271, -7.200742295513424374, -5.783357778048668685 ) ) ;
#8442 = TOROIDAL_SURFACE ( 'NONE', #9030, 10.40000000000000036, 0.9000000000000003553 ) ;
#8443 = EDGE_CURVE ( 'NONE', #15077, #14372, #967, .T. ) ;
#8444 = ORIENTED_EDGE ( 'NONE', *, *, #3385, .F. ) ;
#8445 = ORIENTED_EDGE ( 'NONE', *, *, #5534, .F. ) ;
#8446 = CARTESIAN_POINT ( 'NONE',  ( 26.82912971812489644, -6.258282166232842947, 3.283357778048663356 ) ) ;
#8447 = CARTESIAN_POINT ( 'NONE',  ( 0.000000000000000000, 0.000000000000000000, -4.674599999999997202 ) ) ;
#8448 = AXIS2_PLACEMENT_3D ( 'NONE', #13545, #5359, #8358 ) ;
#8449 = AXIS2_PLACEMENT_3D ( 'NONE', #15991, #6460, #5253 ) ;
#8450 = EDGE_LOOP ( 'NONE', ( #6281, #3158, #3305, #12359 ) ) ;
#8451 = CARTESIAN_POINT ( 'NONE',  ( -27.17934203385504333, -30.00000000000000355, 0.000000000000000000 ) ) ;
#8452 = ORIENTED_EDGE ( 'NONE', *, *, #11091, .T. ) ;
#8453 = CARTESIAN_POINT ( 'NONE',  ( 29.76058531221316272, -5.705227139567997874, -7.939653947423662927 ) ) ;
#8454 = CARTESIAN_POINT ( 'NONE',  ( -20.00000000000000355, 7.999999999999996447, -6.000000000000000000 ) ) ;
#8455 = ORIENTED_EDGE ( 'NONE', *, *, #15520, .T. ) ;
#8456 = ORIENTED_EDGE ( 'NONE', *, *, #1098, .F. ) ;
#8457 = EDGE_CURVE ( 'NONE', #15476, #14976, #1541, .T. ) ;
#8458 = CARTESIAN_POINT ( 'NONE',  ( 29.64681518302145591, -6.972875258987813574, -5.783357778048668685 ) ) ;
#8459 = ADVANCED_FACE ( 'NONE', ( #14484 ), #9204, .F. ) ;
#8460 = DIRECTION ( 'NONE',  ( -0.9928203230275510771, -0.1196152422706609902, -9.614813431917821547E-17 ) ) ;
#8461 = CARTESIAN_POINT ( 'NONE',  ( 41.48299637458987377, 0.4863435510060803435, -5.783357778048662468 ) ) ;
#8462 = ORIENTED_EDGE ( 'NONE', *, *, #14891, .F. ) ;
#8463 = AXIS2_PLACEMENT_3D ( 'NONE', #1152, #8125, #2598 ) ;
#8464 = CARTESIAN_POINT ( 'NONE',  ( 31.75254397038802878, -4.211294393702175398, -8.283357778048662468 ) ) ;
#8465 = AXIS2_PLACEMENT_3D ( 'NONE', #3356, #10314, #7795 ) ;
#8466 = ORIENTED_EDGE ( 'NONE', *, *, #6011, .F. ) ;
#8467 = ORIENTED_EDGE ( 'NONE', *, *, #11942, .F. ) ;
#8468 = CARTESIAN_POINT ( 'NONE',  ( 25.59340017005574097, -5.757764245108966783, 3.283357778048662468 ) ) ;
#8469 = CARTESIAN_POINT ( 'NONE',  ( 25.88156304229571703, -4.918631652813365562, 3.627061608673664228 ) ) ;
#8470 = DIRECTION ( 'NONE',  ( -1.000000000000000000, 0.000000000000000000, 0.000000000000000000 ) ) ;
#8471 = ORIENTED_EDGE ( 'NONE', *, *, #1186, .F. ) ;
#8472 = AXIS2_PLACEMENT_3D ( 'NONE', #418, #9815, #15364 ) ;
#8473 = CARTESIAN_POINT ( 'NONE',  ( 28.83304567166618781, -6.743756660494150346, 4.533357778048659803 ) ) ;
#8474 = VERTEX_POINT ( 'NONE', #10633 ) ;
#8475 = CARTESIAN_POINT ( 'NONE',  ( -2.749999999999992895, -20.49999999999999645, 13.00000000000000178 ) ) ;
#8476 = ORIENTED_EDGE ( 'NONE', *, *, #4941, .T. ) ;
#8477 = DIRECTION ( 'NONE',  ( 1.000000000000000000, 0.000000000000000000, 0.000000000000000000 ) ) ;
#8478 = CARTESIAN_POINT ( 'NONE',  ( 27.00222791626931595, -2.275731535614434531, -5.783357778048658027 ) ) ;
#8479 = DIRECTION ( 'NONE',  ( -0.1196152422706610735, 0.9928203230275511881, 0.000000000000000000 ) ) ;
#8480 = LINE ( 'NONE', #422, #16226 ) ;
#8481 = APPLICATION_PROTOCOL_DEFINITION ( 'draft international standard', 'automotive_design', 1998, #5262 ) ;
#8482 = DIRECTION ( 'NONE',  ( -1.000000000000000000, 0.000000000000000000, 0.000000000000000000 ) ) ;
#8483 = CARTESIAN_POINT ( 'NONE',  ( 25.71748644841968456, -2.420320648352051851, -5.783357778048663356 ) ) ;
#8484 = EDGE_CURVE ( 'NONE', #7158, #14985, #2739, .T. ) ;
#8485 = CARTESIAN_POINT ( 'NONE',  ( 0.000000000000000000, 0.000000000000000000, -12.00000000000000000 ) ) ;
#8486 = LINE ( 'NONE', #12379, #2287 ) ;
#8487 = CARTESIAN_POINT ( 'NONE',  ( 29.77797860222238313, -3.195249460342344250, 7.939653947423664704 ) ) ;
#8488 = ORIENTED_EDGE ( 'NONE', *, *, #16754, .T. ) ;
#8489 = EDGE_CURVE ( 'NONE', #17637, #16432, #7592, .T. ) ;
#8490 = ORIENTED_EDGE ( 'NONE', *, *, #9289, .T. ) ;
#8491 = CARTESIAN_POINT ( 'NONE',  ( 30.02326902268086428, -5.673578940050561847, 7.939653947423658487 ) ) ;
#8492 = CARTESIAN_POINT ( 'NONE',  ( 3.000000000000000000, 0.000000000000000000, 2.399999999999999467 ) ) ;
#8493 = ORIENTED_EDGE ( 'NONE', *, *, #11024, .F. ) ;
#8494 = CARTESIAN_POINT ( 'NONE',  ( -1.500000000000000666, -5.809475019311125976, -3.000000000000000000 ) ) ;
#8495 = CARTESIAN_POINT ( 'NONE',  ( 31.05948030073166066, -1.776715885202022394, -5.783357778048661579 ) ) ;
#8496 = CARTESIAN_POINT ( 'NONE',  ( -16.75000000000000000, -16.21813761408365195, -16.03574476417183448 ) ) ;
#8497 = CIRCLE ( 'NONE', #10785, 0.8999999999999998002 ) ;
#8498 = CARTESIAN_POINT ( 'NONE',  ( 33.23365877489121090, -6.550928303235100891, -5.783357778048663356 ) ) ;
#8499 = CARTESIAN_POINT ( 'NONE',  ( 25.88156304229571703, -4.918631652813365562, -7.939653947423662039 ) ) ;
#8500 = CARTESIAN_POINT ( 'NONE',  ( -20.00000000000000000, 7.999999999999996447, -15.51150668642334374 ) ) ;
#8501 =( BOUNDED_SURFACE ( )  B_SPLINE_SURFACE ( 1, 2, ( 
 ( #7697, #535, #9147, #10225, #1256, #9397, #10654, #990, #12123, #17700, #6681, #1162, #7878, #8223, #13667, #3700, #16225, #6517, #7964, #3795, #2517, #12384, #2608, #15020, #13754, #17871, #9315, #5394, #16480, #6773, #12029, #17951, #1070, #9481, #5485, #17615, #14771, #1334, #5222, #13497, #14854, #8042, #2442, #6592, #9225, #10912, #11006, #2698, #12216, #17790, #16318, #5135, #4051, #16399, #6858, #13580, #10743, #5311, #2359, #9564, #3883, #14938, #13410, #10833, #3966, #8137, #12306, #15113, #3141, #13926, #11173, #8491, #11267, #15559, #242, #9830, #15200, #15380, #1422, #14025, #16746, #1612, #4497, #5575, #8575, #14111, #10012, #8676, #14201, #2965, #1522, #6944, #7142, #12743, #4232, #12653, #7052, #13833, #5753, #12478, #7230, #12567, #149, #3055, #434, #2867, #1796, #7327, #12844, #9731, #64, #5938, #1697, #16845, #341, #15286, #5848, #16568, #11371, #4410, #8393, #16939, #4151, #9650, #4319, #2782, #5662, #11093, #8305, #16658, #9923, #15473, #14305, #10286, #8854, #3602, #14663, #12927, #10204, #1888, #695, #2244, #7415, #4847, #7757, #14389, #9124, #6125, #3501, #6220, #14585, #10376, #15930 ),
 ( #11654, #779, #513, #4760, #13018, #13289, #869, #6026, #17221, #15836, #11556, #9033, #2161, #6308, #17123, #7678, #11828, #10469, #4674, #13203, #8772, #11737, #1973, #3409, #8940, #15751, #11463, #3327, #7495, #17408, #14482, #3234, #604, #2066, #7590, #13115, #17310, #4938, #16031, #15654, #17029, #4583, #10105, #965, #3678, #10631, #13383, #5198, #15090, #5287, #17764, #10889, #2581, #6494, #8108, #1230, #9458, #9202, #2672, #3770, #12185, #8202, #2336, #17510, #16458, #7940, #16205, #17591, #10720, #5111, #12010, #11919, #13640, #13729, #5370, #3861, #9372, #1050, #14749, #6751, #1130, #4026, #16292, #14833, #2493, #9542, #12282, #9292, #7854, #6401, #6656, #3943, #2418, #10805, #13475, #5031, #6571, #10553, #12092, #16379, #14913, #17677, #8016, #13554, #14994, #16118, #17850, #3116, #5460, #13902, #4296, #40, #11243, #15449, #8370, #16918, #14003, #1399, #4474, #10980, #314, #16819, #8281, #11346, #15179, #1493, #4386, #8555, #6920, #7028, #14087, #9988, #16634, #12364, #13811, #9900, #3032, #12720, #1586, #7119, #6833, #1674, #11152, #16724, #4121, #12546, #8649, #17930, #9629, #12454, #8469, #7209, #1312 ) ),
 .UNSPECIFIED., .F., .F., .T. ) 
 B_SPLINE_SURFACE_WITH_KNOTS ( ( 2, 2 ),
 ( 3, 2, 2, 2, 2, 2, 2, 2, 2, 2, 2, 2, 2, 2, 2, 2, 2, 2, 2, 2, 2, 2, 2, 2, 2, 2, 2, 2, 2, 2, 2, 2, 2, 2, 2, 2, 2, 2, 2, 2, 2, 2, 2, 2, 2, 2, 2, 2, 2, 2, 2, 2, 2, 2, 2, 2, 2, 2, 2, 2, 2, 2, 2, 2, 2, 2, 2, 2, 2, 2, 2, 2, 2, 2, 2, 2, 3 ),
 ( 0.000000000000000000, 1.000000000000000000 ),
 ( 0.000000000000000000, 0.01282051282051282007, 0.02564102564102564014, 0.03846153846153846367, 0.05128205128205128027, 0.06410256410256409687, 0.07692307692307692735, 0.08974358974358974395, 0.1025641025641025605, 0.1153846153846153910, 0.1282051282051281937, 0.1410256410256410242, 0.1538461538461538547, 0.1666666666666666574, 0.1794871794871794879, 0.1923076923076923184, 0.2051282051282051211, 0.2179487179487179516, 0.2307692307692307820, 0.2435897435897435848, 0.2564102564102563875, 0.2692307692307692180, 0.2820512820512820484, 0.2948717948717948789, 0.3076923076923077094, 0.3205128205128205399, 0.3333333333333333148, 0.3461538461538461453, 0.3589743589743589758, 0.3717948717948718063, 0.3846153846153846367, 0.3974358974358974117, 0.4102564102564102422, 0.4230769230769230727, 0.4358974358974359031, 0.4487179487179487336, 0.4615384615384615641, 0.4743589743589743390, 0.4871794871794871695, 0.5000000000000000000, 0.5128205128205127750, 0.5256410256410256610, 0.5384615384615384359, 0.5512820512820513219, 0.5641025641025640969, 0.5769230769230768718, 0.5897435897435897578, 0.6025641025641025328, 0.6153846153846154188, 0.6282051282051281937, 0.6410256410256410797, 0.6538461538461538547, 0.6666666666666666297, 0.6794871794871795156, 0.6923076923076922906, 0.7051282051282051766, 0.7179487179487179516, 0.7307692307692307265, 0.7435897435897436125, 0.7564102564102563875, 0.7692307692307692735, 0.7820512820512820484, 0.7948717948717948234, 0.8076923076923077094, 0.8205128205128204844, 0.8333333333333333703, 0.8461538461538461453, 0.8589743589743589203, 0.8717948717948718063, 0.8846153846153845812, 0.8974358974358974672, 0.9102564102564102422, 0.9230769230769231282, 0.9358974358974359031, 0.9487179487179486781, 0.9615384615384615641, 0.9690838366659333403 ),
 .UNSPECIFIED. ) 
 GEOMETRIC_REPRESENTATION_ITEM ( )  RATIONAL_B_SPLINE_SURFACE ( (
 ( 1.000000000000000000, 0.8660254037844387076, 1.000000000000000000, 0.8660254037844387076, 1.000000000000000000, 0.8660254037844387076, 1.000000000000000000, 0.8660254037844387076, 1.000000000000000000, 0.8660254037844387076, 1.000000000000000000, 0.8660254037844387076, 1.000000000000000000, 0.8660254037844387076, 1.000000000000000000, 0.8660254037844387076, 1.000000000000000000, 0.8660254037844387076, 1.000000000000000000, 0.8660254037844387076, 1.000000000000000000, 0.8660254037844387076, 1.000000000000000000, 0.8660254037844387076, 1.000000000000000000, 0.8660254037844387076, 1.000000000000000000, 0.8660254037844387076, 1.000000000000000000, 0.8660254037844387076, 1.000000000000000000, 0.8660254037844387076, 1.000000000000000000, 0.8660254037844387076, 1.000000000000000000, 0.8660254037844387076, 1.000000000000000000, 0.8660254037844387076, 1.000000000000000000, 0.8660254037844387076, 1.000000000000000000, 0.8660254037844387076, 1.000000000000000000, 0.8660254037844387076, 1.000000000000000000, 0.8660254037844387076, 1.000000000000000000, 0.8660254037844387076, 1.000000000000000000, 0.8660254037844387076, 1.000000000000000000, 0.8660254037844387076, 1.000000000000000000, 0.8660254037844387076, 1.000000000000000000, 0.8660254037844387076, 1.000000000000000000, 0.8660254037844387076, 1.000000000000000000, 0.8660254037844387076, 1.000000000000000000, 0.8660254037844387076, 1.000000000000000000, 0.8660254037844387076, 1.000000000000000000, 0.8660254037844387076, 1.000000000000000000, 0.8660254037844387076, 1.000000000000000000, 0.8660254037844387076, 1.000000000000000000, 0.8660254037844387076, 1.000000000000000000, 0.8660254037844387076, 1.000000000000000000, 0.8660254037844387076, 1.000000000000000000, 0.8660254037844387076, 1.000000000000000000, 0.8660254037844387076, 1.000000000000000000, 0.8660254037844387076, 1.000000000000000000, 0.8660254037844387076, 1.000000000000000000, 0.8660254037844387076, 1.000000000000000000, 0.8660254037844387076, 1.000000000000000000, 0.8660254037844387076, 1.000000000000000000, 0.8660254037844387076, 1.000000000000000000, 0.8660254037844387076, 1.000000000000000000, 0.8660254037844387076, 1.000000000000000000, 0.8660254037844387076, 1.000000000000000000, 0.8660254037844387076, 1.000000000000000000, 0.8660254037844387076, 1.000000000000000000, 0.8660254037844387076, 1.000000000000000000, 0.8660254037844387076, 1.000000000000000000, 0.8660254037844387076, 1.000000000000000000, 0.8660254037844387076, 1.000000000000000000, 0.8660254037844387076, 1.000000000000000000, 0.8660254037844387076, 1.000000000000000000, 0.8660254037844387076, 1.000000000000000000, 0.8660254037844387076, 1.000000000000000000, 0.8660254037844387076, 1.000000000000000000, 0.8660254037844387076, 1.000000000000000000, 0.8660254037844387076, 1.000000000000000000, 0.8660254037844387076, 1.000000000000000000, 0.8660254037844387076, 1.000000000000000000, 0.8660254037844387076, 1.000000000000000000, 0.8660254037844387076, 1.000000000000000000, 0.8660254037844387076, 1.000000000000000000, 0.8660254037844387076, 1.000000000000000000, 0.8660254037844387076, 1.000000000000000000, 0.8660254037844387076, 1.000000000000000000, 0.8660254037844387076, 1.000000000000000000, 0.8660254037844387076, 1.000000000000000000, 0.8660254037844387076, 1.000000000000000000, 0.8660254037844387076, 1.000000000000000000, 0.8660254037844387076, 1.000000000000000000, 0.9211506902921580142, 0.9351132093492240394),
 ( 1.000000000000000000, 0.8660254037844387076, 1.000000000000000000, 0.8660254037844387076, 1.000000000000000000, 0.8660254037844387076, 1.000000000000000000, 0.8660254037844387076, 1.000000000000000000, 0.8660254037844387076, 1.000000000000000000, 0.8660254037844387076, 1.000000000000000000, 0.8660254037844387076, 1.000000000000000000, 0.8660254037844387076, 1.000000000000000000, 0.8660254037844387076, 1.000000000000000000, 0.8660254037844387076, 1.000000000000000000, 0.8660254037844387076, 1.000000000000000000, 0.8660254037844387076, 1.000000000000000000, 0.8660254037844387076, 1.000000000000000000, 0.8660254037844387076, 1.000000000000000000, 0.8660254037844387076, 1.000000000000000000, 0.8660254037844387076, 1.000000000000000000, 0.8660254037844387076, 1.000000000000000000, 0.8660254037844387076, 1.000000000000000000, 0.8660254037844387076, 1.000000000000000000, 0.8660254037844387076, 1.000000000000000000, 0.8660254037844387076, 1.000000000000000000, 0.8660254037844387076, 1.000000000000000000, 0.8660254037844387076, 1.000000000000000000, 0.8660254037844387076, 1.000000000000000000, 0.8660254037844387076, 1.000000000000000000, 0.8660254037844387076, 1.000000000000000000, 0.8660254037844387076, 1.000000000000000000, 0.8660254037844387076, 1.000000000000000000, 0.8660254037844387076, 1.000000000000000000, 0.8660254037844387076, 1.000000000000000000, 0.8660254037844387076, 1.000000000000000000, 0.8660254037844387076, 1.000000000000000000, 0.8660254037844387076, 1.000000000000000000, 0.8660254037844387076, 1.000000000000000000, 0.8660254037844387076, 1.000000000000000000, 0.8660254037844387076, 1.000000000000000000, 0.8660254037844387076, 1.000000000000000000, 0.8660254037844387076, 1.000000000000000000, 0.8660254037844387076, 1.000000000000000000, 0.8660254037844387076, 1.000000000000000000, 0.8660254037844387076, 1.000000000000000000, 0.8660254037844387076, 1.000000000000000000, 0.8660254037844387076, 1.000000000000000000, 0.8660254037844387076, 1.000000000000000000, 0.8660254037844387076, 1.000000000000000000, 0.8660254037844387076, 1.000000000000000000, 0.8660254037844387076, 1.000000000000000000, 0.8660254037844387076, 1.000000000000000000, 0.8660254037844387076, 1.000000000000000000, 0.8660254037844387076, 1.000000000000000000, 0.8660254037844387076, 1.000000000000000000, 0.8660254037844387076, 1.000000000000000000, 0.8660254037844387076, 1.000000000000000000, 0.8660254037844387076, 1.000000000000000000, 0.8660254037844387076, 1.000000000000000000, 0.8660254037844387076, 1.000000000000000000, 0.8660254037844387076, 1.000000000000000000, 0.8660254037844387076, 1.000000000000000000, 0.8660254037844387076, 1.000000000000000000, 0.8660254037844387076, 1.000000000000000000, 0.8660254037844387076, 1.000000000000000000, 0.8660254037844387076, 1.000000000000000000, 0.8660254037844387076, 1.000000000000000000, 0.8660254037844387076, 1.000000000000000000, 0.8660254037844387076, 1.000000000000000000, 0.8660254037844387076, 1.000000000000000000, 0.8660254037844387076, 1.000000000000000000, 0.8660254037844387076, 1.000000000000000000, 0.8660254037844387076, 1.000000000000000000, 0.8660254037844387076, 1.000000000000000000, 0.8660254037844387076, 1.000000000000000000, 0.8660254037844387076, 1.000000000000000000, 0.8660254037844387076, 1.000000000000000000, 0.8660254037844387076, 1.000000000000000000, 0.8660254037844387076, 1.000000000000000000, 0.9211506902921580142, 0.9351132093492240394) ) ) 
 REPRESENTATION_ITEM ( '' )  SURFACE ( )  );
#8502 = CARTESIAN_POINT ( 'NONE',  ( 29.30958546476020743, -4.505622649006972402, -8.283357778048662468 ) ) ;
#8503 = CARTESIAN_POINT ( 'NONE',  ( 29.25000000000000000, -16.63088773646508756, 13.37255996287878013 ) ) ;
#8504 = LINE ( 'NONE', #4687, #15340 ) ;
#8505 = CARTESIAN_POINT ( 'NONE',  ( 30.88125018618674744, -3.062327022369072171, -3.627061608673662896 ) ) ;
#8506 = ORIENTED_EDGE ( 'NONE', *, *, #11427, .F. ) ;
#8507 = EDGE_CURVE ( 'NONE', #7462, #12543, #8344, .T. ) ;
#8508 = CARTESIAN_POINT ( 'NONE',  ( 26.01345249736710841, -4.876873030332669501, -8.181274557237335543 ) ) ;
#8509 = FACE_OUTER_BOUND ( 'NONE', #16440, .T. ) ;
#8510 = ORIENTED_EDGE ( 'NONE', *, *, #5987, .T. ) ;
#8511 = ORIENTED_EDGE ( 'NONE', *, *, #1321, .T. ) ;
#8512 = EDGE_CURVE ( 'NONE', #16561, #12534, #7133, .T. ) ;
#8513 = VERTEX_POINT ( 'NONE', #7680 ) ;
#8514 = ORIENTED_EDGE ( 'NONE', *, *, #10326, .T. ) ;
#8515 = CARTESIAN_POINT ( 'NONE',  ( 28.36401332423200827, -6.500457016816879374, 4.705209693361160461 ) ) ;
#8516 = CARTESIAN_POINT ( 'NONE',  ( 25.90934487712387480, 0.1208734971681841297, 15.78335777804866424 ) ) ;
#8517 = CARTESIAN_POINT ( 'NONE',  ( 2.100000000000000089, 0.000000000000000000, 1.159999999999999476 ) ) ;
#8518 = CARTESIAN_POINT ( 'NONE',  ( 10.50000000000000000, 1.285879139104720831E-15, -6.005572809000082835 ) ) ;
#8519 = LINE ( 'NONE', #1640, #1206 ) ;
#8520 = CARTESIAN_POINT ( 'NONE',  ( 30.78070346053490880, -6.209293581256383199, -4.705209693361168455 ) ) ;
#8521 = CARTESIAN_POINT ( 'NONE',  ( 29.62480591732145996, -4.467644809586046151, -3.283357778048664688 ) ) ;
#8522 = DIRECTION ( 'NONE',  ( -0.1196152422706610041, 0.9928203230275510771, 0.000000000000000000 ) ) ;
#8523 = LINE ( 'NONE', #16970, #13665 ) ;
#8524 =( BOUNDED_CURVE ( )  B_SPLINE_CURVE ( 3, ( #6556, #9360, #1036, #13459 ),
 .UNSPECIFIED., .F., .T. ) 
 B_SPLINE_CURVE_WITH_KNOTS ( ( 4, 4 ),
 ( 4.774018107371971631, 4.846194975958193929 ),
 .UNSPECIFIED. ) 
 CURVE ( )  GEOMETRIC_REPRESENTATION_ITEM ( )  RATIONAL_B_SPLINE_CURVE ( ( 1.000000000000000000, 0.9995659220841806025, 0.9995659220841806025, 1.000000000000000000 ) ) 
 REPRESENTATION_ITEM ( '' )  );
#8525 = CARTESIAN_POINT ( 'NONE',  ( 26.58890374069123652, -3.379597482641427231, -8.283357778048658915 ) ) ;
#8526 = ORIENTED_EDGE ( 'NONE', *, *, #16853, .T. ) ;
#8527 = EDGE_CURVE ( 'NONE', #947, #15308, #14555, .T. ) ;
#8528 = CARTESIAN_POINT ( 'NONE',  ( 30.67110321781257909, -3.087645581983020637, -7.939653947423660263 ) ) ;
#8529 = DIRECTION ( 'NONE',  ( 1.000000000000000000, 0.000000000000000000, -0.000000000000000000 ) ) ;
#8530 = CARTESIAN_POINT ( 'NONE',  ( 26.01652455409633902, -4.902371455920928156, -5.783357778048663356 ) ) ;
#8531 = DIRECTION ( 'NONE',  ( -0.000000000000000000, -0.000000000000000000, 1.000000000000000000 ) ) ;
#8532 =( REPRESENTATION_RELATIONSHIP ('NONE','NONE', #3227, #2651 ) REPRESENTATION_RELATIONSHIP_WITH_TRANSFORMATION ( #16017 )SHAPE_REPRESENTATION_RELATIONSHIP( ) );
#8533 = DIRECTION ( 'NONE',  ( 0.000000000000000000, 0.000000000000000000, 1.000000000000000000 ) ) ;
#8534 = CARTESIAN_POINT ( 'NONE',  ( 30.54048978798443059, -6.538043363838207611, 7.033357778048657138 ) ) ;
#8535 = CARTESIAN_POINT ( 'NONE',  ( 12.70000000000000284, 1.555301434917138827E-15, 0.000000000000000000 ) ) ;
#8536 = ORIENTED_EDGE ( 'NONE', *, *, #17191, .F. ) ;
#8537 = ORIENTED_EDGE ( 'NONE', *, *, #14655, .F. ) ;
#8538 = CARTESIAN_POINT ( 'NONE',  ( 26.56758885001203652, -2.317900097157796324, 5.783357778048657138 ) ) ;
#8539 = DIRECTION ( 'NONE',  ( 0.9237280213470681067, 0.3830490080632377170, 0.000000000000000000 ) ) ;
#8540 = EDGE_CURVE ( 'NONE', #9208, #1330, #16403, .T. ) ;
#8541 = DIRECTION ( 'NONE',  ( 0.000000000000000000, 0.000000000000000000, 1.000000000000000000 ) ) ;
#8542 = ORIENTED_EDGE ( 'NONE', *, *, #1611, .T. ) ;
#8543 = CARTESIAN_POINT ( 'NONE',  ( 27.78610916120306129, -6.570083055755264745, -4.705209693361169343 ) ) ;
#8544 = EDGE_LOOP ( 'NONE', ( #11945, #5104, #6728, #3160, #4739 ) ) ;
#8545 = ADVANCED_FACE ( 'NONE', ( #350 ), #5859, .F. ) ;
#8546 = CARTESIAN_POINT ( 'NONE',  ( 31.53813789838894621, -6.745008222462202774, -5.783357778048668685 ) ) ;
#8547 = EDGE_CURVE ( 'NONE', #3640, #1158, #13691, .T. ) ;
#8548 = FACE_OUTER_BOUND ( 'NONE', #3742, .T. ) ;
#8549 = CARTESIAN_POINT ( 'NONE',  ( 33.60446413004628141, -3.988174587000466342, -3.627061608673664672 ) ) ;
#8550 = CARTESIAN_POINT ( 'NONE',  ( 33.06225340847440464, -6.234220648470727433, -4.533357778048668685 ) ) ;
#8551 = CARTESIAN_POINT ( 'NONE',  ( 16.79145860028663151, -17.04903085677362640, -16.02982020200856184 ) ) ;
#8552 = ORIENTED_EDGE ( 'NONE', *, *, #8965, .T. ) ;
#8553 = CARTESIAN_POINT ( 'NONE',  ( 32.77257290155422709, -2.834459985843461816, 7.939653947423664704 ) ) ;
#8554 = EDGE_CURVE ( 'NONE', #14154, #16037, #15851, .T. ) ;
#8555 = CARTESIAN_POINT ( 'NONE',  ( 27.23882169172318513, -6.009049854935478052, 3.627061608673662896 ) ) ;
#8556 = CARTESIAN_POINT ( 'NONE',  ( -29.04317620846695647, -17.86624673319742840, 13.43120144060744003 ) ) ;
#8557 = CARTESIAN_POINT ( 'NONE',  ( 13.00000000000000178, 0.000000000000000000, 12.00000000000000000 ) ) ;
#8558 = ORIENTED_EDGE ( 'NONE', *, *, #6767, .F. ) ;
#8559 = PRESENTATION_STYLE_ASSIGNMENT (( #9905 ) ) ;
#8560 = VERTEX_POINT ( 'NONE', #8584 ) ;
#8561 = CARTESIAN_POINT ( 'NONE',  ( -45.50000000000000000, -16.03270077640482683, -5.537981825772250843 ) ) ;
#8562 = VERTEX_POINT ( 'NONE', #14034 ) ;
#8563 = CARTESIAN_POINT ( 'NONE',  ( 0.000000000000000000, 0.000000000000000000, -10.47749643873921244 ) ) ;
#8564 = CARTESIAN_POINT ( 'NONE',  ( 33.64386668575551198, -3.983427357176565486, -8.283357778048662468 ) ) ;
#8565 = CARTESIAN_POINT ( 'NONE',  ( 33.40745134805642635, -4.011910736534825439, -3.283357778048664688 ) ) ;
#8566 = DIRECTION ( 'NONE',  ( -0.000000000000000000, -0.000000000000000000, -1.000000000000000000 ) ) ;
#8567 = CYLINDRICAL_SURFACE ( 'NONE', #11548, 5.500000000000000888 ) ;
#8568 = CARTESIAN_POINT ( 'NONE',  ( 33.35047706458318828, -2.764833946905071560, -7.939653947423660263 ) ) ;
#8569 = CARTESIAN_POINT ( 'NONE',  ( 1.746467850512308208E-21, -1.591841644184202181E-21, -6.005572809000082835 ) ) ;
#8570 = CARTESIAN_POINT ( 'NONE',  ( 26.90109536843240789, -7.313877135454839973, -5.113484796970856117 ) ) ;
#8571 = CARTESIAN_POINT ( 'NONE',  ( 30.40841950734487753, -3.119293781500474427, 7.939653947423664704 ) ) ;
#8572 = ORIENTED_EDGE ( 'NONE', *, *, #14, .T. ) ;
#8573 = EDGE_LOOP ( 'NONE', ( #8891, #4846, #5272, #16291 ) ) ;
#8574 = EDGE_CURVE ( 'NONE', #6239, #6149, #16856, .T. ) ;
#8575 = CARTESIAN_POINT ( 'NONE',  ( 29.19137779418881351, -4.519864338893556877, 7.939653947423662039 ) ) ;
#8576 = DIRECTION ( 'NONE',  ( 0.9928203230275510771, 0.1196152422706609902, 4.006172263299092517E-17 ) ) ;
#8577 = DIRECTION ( 'NONE',  ( -0.000000000000000000, -0.000000000000000000, 1.000000000000000000 ) ) ;
#8578 = ADVANCED_FACE ( 'NONE', ( #4507, #4420 ), #1623, .F. ) ;
#8579 = ORIENTED_EDGE ( 'NONE', *, *, #9764, .F. ) ;
#8580 = PLANE ( 'NONE',  #16353 ) ;
#8581 = CARTESIAN_POINT ( 'NONE',  ( 46.37688276194213444, -2.449350377220338881, -5.783357778048662468 ) ) ;
#8582 = DIRECTION ( 'NONE',  ( 1.000000000000000000, 1.776356839400250465E-15, 0.000000000000000000 ) ) ;
#8583 = CARTESIAN_POINT ( 'NONE',  ( 32.93832978346670615, -1.887710243310447567, -7.033357778048658027 ) ) ;
#8584 = CARTESIAN_POINT ( 'NONE',  ( -45.00000000000000711, -19.03270077640482683, 10.53798182577225084 ) ) ;
#8585 = CARTESIAN_POINT ( 'NONE',  ( 28.20260476654369697, -6.819712339336020612, -7.033357778048666908 ) ) ;
#8586 = CARTESIAN_POINT ( 'NONE',  ( 29.20951391065003122, -17.04067956308641030, 13.38411038749911697 ) ) ;
#8587 = CARTESIAN_POINT ( 'NONE',  ( 25.71748644841968456, -2.420320648352046078, 5.783357778048663356 ) ) ;
#8588 = EDGE_CURVE ( 'NONE', #5981, #16863, #4230, .T. ) ;
#8589 = SURFACE_STYLE_FILL_AREA ( #14401 ) ;
#8590 = CARTESIAN_POINT ( 'NONE',  ( 31.28415083292585663, -5.521667582366822202, -3.627061608673667781 ) ) ;
#8591 = CARTESIAN_POINT ( 'NONE',  ( 26.41562710823574278, -3.600346414165641828, -7.939653947423660263 ) ) ;
#8592 = LINE ( 'NONE', #14224, #261 ) ;
#8593 = B_SPLINE_CURVE_WITH_KNOTS ( 'NONE', 3,
 ( #17202, #11810, #17389, #16009, #4745, #4922, #8923, #2143, #2044, #11721, #15910, #7570, #2228, #13097, #17291, #10450 ),
 .UNSPECIFIED., .F., .F.,
 ( 4, 2, 2, 2, 2, 2, 2, 4 ),
 ( 0.000000000000000000, 0.0008414457502979328513, 0.001262168625446899277, 0.001682891500595865703, 0.002103614375744832128, 0.002524337250893798554, 0.002945060126042764979, 0.003365783001191731405 ),
 .UNSPECIFIED. ) ;
#8594 = ORIENTED_EDGE ( 'NONE', *, *, #1804, .F. ) ;
#8595 = ORIENTED_EDGE ( 'NONE', *, *, #16722, .F. ) ;
#8596 = CARTESIAN_POINT ( 'NONE',  ( 31.59864285835955400, -2.049116061056871274, -7.033357778048658027 ) ) ;
#8597 = ORIENTED_EDGE ( 'NONE', *, *, #15378, .T. ) ;
#8598 = ORIENTED_EDGE ( 'NONE', *, *, #12117, .T. ) ;
#8599 = CARTESIAN_POINT ( 'NONE',  ( 27.93049598394382116, -4.671775696577297410, 7.939653947423662039 ) ) ;
#8600 = B_SPLINE_CURVE_WITH_KNOTS ( 'NONE', 3,
 ( #9281, #8009, #13548, #17754, #9536, #14821 ),
 .UNSPECIFIED., .F., .F.,
 ( 4, 2, 4 ),
 ( 0.000000000000000000, 0.0002095117440854733380, 0.0004190234881709466760 ),
 .UNSPECIFIED. ) ;
#8601 = FACE_OUTER_BOUND ( 'NONE', #2441, .T. ) ;
#8602 = CYLINDRICAL_SURFACE ( 'NONE', #17655, 6.249999999999998224 ) ;
#8603 = EDGE_CURVE ( 'NONE', #15926, #6798, #15250, .T. ) ;
#8604 = CARTESIAN_POINT ( 'NONE',  ( -17.24286622940504188, 11.12094428624988218, -15.96573730347181019 ) ) ;
#8605 = CARTESIAN_POINT ( 'NONE',  ( -20.00000000000000000, 7.999999999999996447, -6.000000000000000000 ) ) ;
#8606 = CARTESIAN_POINT ( 'NONE',  ( 32.04575515724926760, -1.668086104879473730, -5.783357778048658027 ) ) ;
#8607 = CARTESIAN_POINT ( 'NONE',  ( 31.74131510559286085, -5.666460835049167422, -3.283357778048667797 ) ) ;
#8608 = LINE ( 'NONE', #5789, #12184 ) ;
#8609 = CARTESIAN_POINT ( 'NONE',  ( 4.000000000000000000, -2.309401076758510918, -4.700000000000000178 ) ) ;
#8610 = UNCERTAINTY_MEASURE_WITH_UNIT (LENGTH_MEASURE( 1.000000000000000082E-05 ), #13425, 'distance_accuracy_value', 'NONE');
#8611 = CARTESIAN_POINT ( 'NONE',  ( 26.18945719470476163, -6.341381504099093291, -7.820351782355674963 ) ) ;
#8612 = EDGE_CURVE ( 'NONE', #14557, #1012, #14440, .T. ) ;
#8613 = CARTESIAN_POINT ( 'NONE',  ( 28.76238721243587193, -5.825490297734302381, -3.627061608673667781 ) ) ;
#8614 = CARTESIAN_POINT ( 'NONE',  ( 31.31418170428987224, -6.782187383561751659, -5.113484796970860558 ) ) ;
#8615 = LINE ( 'NONE', #7955, #12513 ) ;
#8616 = FACE_OUTER_BOUND ( 'NONE', #17476, .T. ) ;
#8617 = EDGE_LOOP ( 'NONE', ( #728, #2242, #5049, #17411, #3201 ) ) ;
#8618 = DIRECTION ( 'NONE',  ( -0.9396926207859143121, 0.000000000000000000, -0.3420201433256525592 ) ) ;
#8619 = CIRCLE ( 'NONE', #16723, 10.50000000000000000 ) ;
#8620 = CARTESIAN_POINT ( 'NONE',  ( 28.60033944477555323, -4.591072787911525843, 3.283357778048664244 ) ) ;
#8621 = FACE_OUTER_BOUND ( 'NONE', #7127, .T. ) ;
#8622 = ORIENTED_EDGE ( 'NONE', *, *, #7647, .F. ) ;
#8623 = ORIENTED_EDGE ( 'NONE', *, *, #2701, .T. ) ;
#8624 = AXIS2_PLACEMENT_3D ( 'NONE', #6510, #7367, #11935 ) ;
#8625 = CYLINDRICAL_SURFACE ( 'NONE', #11968, 10.50000000000000000 ) ;
#8626 = CARTESIAN_POINT ( 'NONE',  ( 35.19141017012124451, -14.17387298022714326, -11.46934516270796323 ) ) ;
#8627 = EDGE_CURVE ( 'NONE', #12549, #5172, #17140, .T. ) ;
#8628 = VERTEX_POINT ( 'NONE', #7598 ) ;
#8629 = CARTESIAN_POINT ( 'NONE',  ( -22.21636613273916794, -10.00424398458219066, -15.08813622000165466 ) ) ;
#8630 = ORIENTED_EDGE ( 'NONE', *, *, #1079, .T. ) ;
#8631 = VECTOR ( 'NONE', #11763, 1000.000000000000000 ) ;
#8632 = CARTESIAN_POINT ( 'NONE',  ( 10.50000000000000000, 1.285879139104720831E-15, -10.00000000000000000 ) ) ;
#8633 = VECTOR ( 'NONE', #14250, 1000.000000000000000 ) ;
#8634 = EDGE_CURVE ( 'NONE', #29, #6646, #5039, .T. ) ;
#8635 = CARTESIAN_POINT ( 'NONE',  ( 31.38469755857769528, -2.374701023479507178, -4.705209693361161349 ) ) ;
#8636 = CARTESIAN_POINT ( 'NONE',  ( -31.74999999999995737, 0.000000000000000000, 0.000000000000000000 ) ) ;
#8637 = CARTESIAN_POINT ( 'NONE',  ( 29.98885399772409954, -6.604504582617394703, 7.033357778048657138 ) ) ;
#8638 = LINE ( 'NONE', #663, #13252 ) ;
#8639 = ORIENTED_EDGE ( 'NONE', *, *, #15322, .F. ) ;
#8640 = CARTESIAN_POINT ( 'NONE',  ( 33.10345976029034176, -2.594722134608779207, -3.283357778048662023 ) ) ;
#8641 = EDGE_CURVE ( 'NONE', #15612, #17048, #14593, .T. ) ;
#8642 = CARTESIAN_POINT ( 'NONE',  ( 29.11066736118121767, -3.075774767273946608, -8.283357778048660691 ) ) ;
#8643 = ORIENTED_EDGE ( 'NONE', *, *, #15743, .T. ) ;
#8644 = CARTESIAN_POINT ( 'NONE',  ( 32.16857880351144416, -6.669052543620333395, 5.783357778048658027 ) ) ;
#8645 = VECTOR ( 'NONE', #4036, 1000.000000000000227 ) ;
#8646 = B_SPLINE_CURVE_WITH_KNOTS ( 'NONE', 3,
 ( #12507, #13454, #5092, #10697 ),
 .UNSPECIFIED., .F., .F.,
 ( 4, 4 ),
 ( 2.843119637691541009E-07, 0.001422633878257849012 ),
 .UNSPECIFIED. ) ;
#8647 = ORIENTED_EDGE ( 'NONE', *, *, #15646, .T. ) ;
#8648 = ADVANCED_FACE ( 'NONE', ( #13297 ), #7504, .T. ) ;
#8649 = CARTESIAN_POINT ( 'NONE',  ( 25.86833963875586306, -3.039313213345869791, 6.861505862736166250 ) ) ;
#8650 = CARTESIAN_POINT ( 'NONE',  ( -16.79042544672876858, -17.04069398696883297, 16.02996823657058911 ) ) ;
#8651 = CARTESIAN_POINT ( 'NONE',  ( -12.50000000000000000, 0.000000000000000000, -4.000000000000000000 ) ) ;
#8652 = ORIENTED_EDGE ( 'NONE', *, *, #7764, .F. ) ;
#8653 = FACE_OUTER_BOUND ( 'NONE', #11462, .T. ) ;
#8654 = CIRCLE ( 'NONE', #9779, 9.500000000000001776 ) ;
#8655 = ORIENTED_EDGE ( 'NONE', *, *, #17282, .T. ) ;
#8656 = CARTESIAN_POINT ( 'NONE',  ( 26.94172295629870462, -6.971623697019761146, 4.533357778048659803 ) ) ;
#8657 = VERTEX_POINT ( 'NONE', #4855 ) ;
#8658 = CARTESIAN_POINT ( 'NONE',  ( 29.71979337562451207, -1.938121702948446323, -5.783357778048664244 ) ) ;
#8659 = CARTESIAN_POINT ( 'NONE',  ( 28.54354359905709870, -7.105797696961086096, -5.783357778048669573 ) ) ;
#8660 = CARTESIAN_POINT ( 'NONE',  ( 33.21234388421201089, -5.489230917751459771, -8.283357778048662468 ) ) ;
#8661 = CARTESIAN_POINT ( 'NONE',  ( -4.000000000000000000, 0.9868501483902580862, -0.09357334158579672101 ) ) ;
#8662 = CARTESIAN_POINT ( 'NONE',  ( -1.527916156725210981E-16, -20.49999999999999645, 17.69999999999999574 ) ) ;
#8663 = PLANE ( 'NONE',  #13303 ) ;
#8664 = CARTESIAN_POINT ( 'NONE',  ( 28.71854711534694715, -4.576831098024959132, -3.627061608673664672 ) ) ;
#8665 = CARTESIAN_POINT ( 'NONE',  ( 33.21234388421201800, -5.489230917751459771, -8.283357778048664244 ) ) ;
#8666 = EDGE_CURVE ( 'NONE', #13857, #12121, #12253, .T. ) ;
#8667 = CARTESIAN_POINT ( 'NONE',  ( 26.01652455409633902, -4.902371455920926380, 5.783357778048663356 ) ) ;
#8668 = CARTESIAN_POINT ( 'NONE',  ( 30.98067518586950442, -1.786210345264705790, -5.783357778048658027 ) ) ;
#8669 = CARTESIAN_POINT ( 'NONE',  ( 29.54591158530375239, -2.596238420101622868, 4.705209693361168455 ) ) ;
#8670 = AXIS2_PLACEMENT_3D ( 'NONE', #5744, #12560, #10002 ) ;
#8671 = VERTEX_POINT ( 'NONE', #3509 ) ;
#8672 = VECTOR ( 'NONE', #6801, 1000.000000000000000 ) ;
#8673 = CARTESIAN_POINT ( 'NONE',  ( 26.99805802979993885, -6.665027654307603022, -4.705209693361168455 ) ) ;
#8674 = VERTEX_POINT ( 'NONE', #703 ) ;
#8675 = EDGE_CURVE ( 'NONE', #11660, #4375, #8335, .T. ) ;
#8676 = CARTESIAN_POINT ( 'NONE',  ( 28.73594040535616756, -2.066853418799292630, 5.783357778048668685 ) ) ;
#8677 = DIRECTION ( 'NONE',  ( -1.000000000000000000, -0.000000000000000000, -0.000000000000000000 ) ) ;
#8678 = CARTESIAN_POINT ( 'NONE',  ( 26.01652455409633902, -4.902371455920926380, -5.783357778048663356 ) ) ;
#8679 = ADVANCED_FACE ( 'NONE', ( #17600 ), #16300, .F. ) ;
#8680 = ORIENTED_EDGE ( 'NONE', *, *, #11541, .F. ) ;
#8681 = CARTESIAN_POINT ( 'NONE',  ( 27.91310269393460430, -7.181753375802955475, 5.783357778048657138 ) ) ;
#8682 = CARTESIAN_POINT ( 'NONE',  ( -4.204114099329565590, 1.660341531092949685, -3.302132361967891061 ) ) ;
#8683 = LINE ( 'NONE', #11379, #16860 ) ;
#8684 = FACE_OUTER_BOUND ( 'NONE', #3212, .T. ) ;
#8685 = AXIS2_PLACEMENT_3D ( 'NONE', #3069, #5768, #15573 ) ;
#8686 = VECTOR ( 'NONE', #9350, 1000.000000000000000 ) ;
#8687 = CARTESIAN_POINT ( 'NONE',  ( 26.97551107961034944, -7.694459687869362519, -5.783357778048669573 ) ) ;
#8688 = DIRECTION ( 'NONE',  ( -0.4999999999999981126, 0.8660254037844397068, 0.000000000000000000 ) ) ;
#8689 = CARTESIAN_POINT ( 'NONE',  ( -15.92260893619738837, -28.39189527176317540, 0.000000000000000000 ) ) ;
#8690 = CARTESIAN_POINT ( 'NONE',  ( 30.88577694472199298, -6.196634301449400084, -6.861505862736166250 ) ) ;
#8691 = VERTEX_POINT ( 'NONE', #2007 ) ;
#8692 = AXIS2_PLACEMENT_3D ( 'NONE', #13909, #1237, #16641 ) ;
#8693 = EDGE_CURVE ( 'NONE', #1377, #2104, #9957, .T. ) ;
#8694 = CARTESIAN_POINT ( 'NONE',  ( 26.52522735095806894, -6.721994413439005278, -4.705209693361169343 ) ) ;
#8695 = CARTESIAN_POINT ( 'NONE',  ( 30.61929490284659394, -6.528548903775525325, -4.533357778048668685 ) ) ;
#8696 = VERTEX_POINT ( 'NONE', #6165 ) ;
#8697 = ORIENTED_EDGE ( 'NONE', *, *, #6725, .F. ) ;
#8698 = ORIENTED_EDGE ( 'NONE', *, *, #6148, .F. ) ;
#8699 = CARTESIAN_POINT ( 'NONE',  ( 27.72904566057427189, -3.442105416578421284, 7.939653947423662927 ) ) ;
#8700 = DIRECTION ( 'NONE',  ( 0.9928203230275511881, 0.1196152422706609764, 1.201851678989727817E-16 ) ) ;
#8701 = CARTESIAN_POINT ( 'NONE',  ( 33.48062616923409252, 0.02583177435456097265, 5.783357778048664244 ) ) ;
#8702 = AXIS2_PLACEMENT_3D ( 'NONE', #13524, #16167, #17731 ) ;
#8703 = CARTESIAN_POINT ( 'NONE',  ( 31.26353094466156080, -6.788289799823394866, 5.783357778048664244 ) ) ;
#8704 = CARTESIAN_POINT ( 'NONE',  ( -23.43613571611706803, -22.46619466838626877, -14.83130101496670861 ) ) ;
#8705 = CARTESIAN_POINT ( 'NONE',  ( 32.72003615946069743, -2.840789625746940938, -7.939653947423660263 ) ) ;
#8706 = CARTESIAN_POINT ( 'NONE',  ( 31.66176685062031027, -1.704152250161192539, -6.453230759126468818 ) ) ;
#8707 = CYLINDRICAL_SURFACE ( 'NONE', #5226, 2.500000000000000000 ) ;
#8708 = CARTESIAN_POINT ( 'NONE',  ( -5.499998387031001634, -20.49508120620799900, 13.00000000000000178 ) ) ;
#8709 = MECHANICAL_DESIGN_GEOMETRIC_PRESENTATION_REPRESENTATION (  '', ( #2627 ), #2900 ) ;
#8710 = CARTESIAN_POINT ( 'NONE',  ( 0.000000000000000000, 0.000000000000000000, 1.599999999999999423 ) ) ;
#8711 = AXIS2_PLACEMENT_3D ( 'NONE', #10621, #3488, #7666 ) ;
#8712 = ORIENTED_EDGE ( 'NONE', *, *, #2478, .T. ) ;
#8713 = CARTESIAN_POINT ( 'NONE',  ( 31.49429780130001433, -5.496349022752856861, -7.939653947423664704 ) ) ;
#8714 = PLANE ( 'NONE',  #3203 ) ;
#8715 = PLANE ( 'NONE',  #17769 ) ;
#8716 = DIRECTION ( 'NONE',  ( 0.000000000000000000, 0.000000000000000000, 1.000000000000000000 ) ) ;
#8717 = CARTESIAN_POINT ( 'NONE',  ( -7.499998387031003411, -20.49508120620799900, -6.000000000000000000 ) ) ;
#8718 = EDGE_CURVE ( 'NONE', #1869, #13908, #6745, .T. ) ;
#8719 = MECHANICAL_DESIGN_GEOMETRIC_PRESENTATION_REPRESENTATION (  '', ( #4649 ), #5511 ) ;
#8720 = CARTESIAN_POINT ( 'NONE',  ( 27.49335874655903567, -6.905162478240574053, 4.533357778048659803 ) ) ;
#8721 = DIRECTION ( 'NONE',  ( 0.9928203230275512992, 0.1196152422706610180, 4.006172263299093133E-17 ) ) ;
#8722 = ORIENTED_EDGE ( 'NONE', *, *, #3576, .F. ) ;
#8723 = ADVANCED_FACE ( 'NONE', ( #464 ), #5869, .T. ) ;
#8724 = AXIS2_PLACEMENT_3D ( 'NONE', #3818, #14704, #12049 ) ;
#8725 = FACE_OUTER_BOUND ( 'NONE', #10604, .T. ) ;
#8726 = ORIENTED_EDGE ( 'NONE', *, *, #3564, .T. ) ;
#8727 = LINE ( 'NONE', #16987, #3489 ) ;
#8728 = ORIENTED_EDGE ( 'NONE', *, *, #10540, .T. ) ;
#8729 = AXIS2_PLACEMENT_3D ( 'NONE', #10752, #14947, #4060 ) ;
#8730 = CARTESIAN_POINT ( 'NONE',  ( 25.71748644841968456, -2.420320648352051851, -5.783357778048663356 ) ) ;
#8731 = CARTESIAN_POINT ( 'NONE',  ( 27.02414796481377124, -2.900061135469103490, -6.861505862736158257 ) ) ;
#8732 = EDGE_LOOP ( 'NONE', ( #6176, #1679, #14756, #13160, #6759, #5871 ) ) ;
#8733 = ORIENTED_EDGE ( 'NONE', *, *, #7066, .F. ) ;
#8734 = CARTESIAN_POINT ( 'NONE',  ( 29.50659824675005893, -4.481886499472614638, -7.939653947423662039 ) ) ;
#8735 = CARTESIAN_POINT ( 'NONE',  ( -10.27627944162877505, 4.200961894323461010, -3.000000000000000888 ) ) ;
#8736 = CARTESIAN_POINT ( 'NONE',  ( 33.18300801526289234, -6.557030719496743210, -6.453230759126470595 ) ) ;
#8737 = PLANE ( 'NONE',  #7754 ) ;
#8738 = CONICAL_SURFACE ( 'NONE', #10453, 3.999999999999998224, 0.8911886515913775009 ) ;
#8739 = ORIENTED_EDGE ( 'NONE', *, *, #16999, .F. ) ;
#8740 = CARTESIAN_POINT ( 'NONE',  ( 32.06776442294927421, -4.173316554281249147, -3.283357778048664688 ) ) ;
#8741 = ADVANCED_FACE ( 'NONE', ( #3172 ), #7442, .F. ) ;
#8742 = CARTESIAN_POINT ( 'NONE',  ( 29.40036258452792950, -7.012764792547963033, -6.453230759126474148 ) ) ;
#8743 = VECTOR ( 'NONE', #11380, 1000.000000000000114 ) ;
#8744 = CARTESIAN_POINT ( 'NONE',  ( 31.88814493096863956, -1.687075024589942851, 5.783357778048668685 ) ) ;
#8745 = VECTOR ( 'NONE', #377, 999.9999999999998863 ) ;
#8746 = EDGE_CURVE ( 'NONE', #16745, #13121, #4432, .T. ) ;
#8747 = CARTESIAN_POINT ( 'NONE',  ( -4.154094228333307548, 2.398367420968273489, -3.421909803043222897 ) ) ;
#8748 = CARTESIAN_POINT ( 'NONE',  ( -22.62145100412528009, -22.46994790986326151, 15.00472644746570694 ) ) ;
#8749 = LINE ( 'NONE', #411, #8074 ) ;
#8750 = AXIS2_PLACEMENT_3D ( 'NONE', #8144, #13674, #9151 ) ;
#8751 = EDGE_LOOP ( 'NONE', ( #17194, #2837, #12747, #1143, #12287 ) ) ;
#8752 = DIRECTION ( 'NONE',  ( 0.000000000000000000, 0.000000000000000000, -1.000000000000000000 ) ) ;
#8753 = ORIENTED_EDGE ( 'NONE', *, *, #3875, .T. ) ;
#8754 = LINE ( 'NONE', #11353, #8986 ) ;
#8755 = DIRECTION ( 'NONE',  ( -0.000000000000000000, -0.000000000000000000, 1.000000000000000000 ) ) ;
#8756 = ORIENTED_EDGE ( 'NONE', *, *, #9257, .F. ) ;
#8757 = CARTESIAN_POINT ( 'NONE',  ( 27.55969062878875064, -7.234529412811931515, -5.783357778048668685 ) ) ;
#8758 = AXIS2_PLACEMENT_3D ( 'NONE', #5568, #7318, #12647 ) ;
#8759 = AXIS2_PLACEMENT_3D ( 'NONE', #16611, #1560, #2649 ) ;
#8760 = CARTESIAN_POINT ( 'NONE',  ( 32.64947922571280259, -7.010858578292532783, -5.783357778048669573 ) ) ;
#8761 = DIRECTION ( 'NONE',  ( 0.000000000000000000, 0.000000000000000000, -1.000000000000000000 ) ) ;
#8762 = APPLICATION_PROTOCOL_DEFINITION ( 'draft international standard', 'automotive_design', 1998, #14562 ) ;
#8763 = FACE_OUTER_BOUND ( 'NONE', #1521, .T. ) ;
#8764 = CARTESIAN_POINT ( 'NONE',  ( 33.26181313012506280, -6.547536259434060923, -6.453230759126471483 ) ) ;
#8765 = CARTESIAN_POINT ( 'NONE',  ( 25.71748644841968456, -2.420320648352051851, -5.783357778048663356 ) ) ;
#8766 = CYLINDRICAL_SURFACE ( 'NONE', #6020, 2.499999999999999112 ) ;
#8767 = CARTESIAN_POINT ( 'NONE',  ( 31.43723430067123914, -2.368371383576012956, 4.705209693361168455 ) ) ;
#8768 = EDGE_LOOP ( 'NONE', ( #699, #10302, #14912, #2381 ) ) ;
#8769 = AXIS2_PLACEMENT_3D ( 'NONE', #11837, #4854, #9040 ) ;
#8770 = CARTESIAN_POINT ( 'NONE',  ( 26.03917326857634151, -4.899642733102906433, -3.627061608673664672 ) ) ;
#8771 = ORIENTED_EDGE ( 'NONE', *, *, #12351, .F. ) ;
#8772 = CARTESIAN_POINT ( 'NONE',  ( 32.93470988637010066, -5.949778345213319497, 4.705209693361159573 ) ) ;
#8773 = LINE ( 'NONE', #11557, #15093 ) ;
#8774 = CARTESIAN_POINT ( 'NONE',  ( 26.32044349065828115, -7.243571858916999950, -6.694428052743685242 ) ) ;
#8775 = ORIENTED_EDGE ( 'NONE', *, *, #3042, .F. ) ;
#8776 = CARTESIAN_POINT ( 'NONE',  ( -4.000000000000000000, -0.8382426107201325083, -2.920612530944983298 ) ) ;
#8777 = EDGE_CURVE ( 'NONE', #6631, #11016, #545, .T. ) ;
#8778 = FACE_OUTER_BOUND ( 'NONE', #12879, .T. ) ;
#8779 = CARTESIAN_POINT ( 'NONE',  ( 25.92467471225709374, -2.732717170633701453, -7.033357778048658027 ) ) ;
#8780 =( BOUNDED_CURVE ( )  B_SPLINE_CURVE ( 2, ( #15686, #4704, #4880, #7704, #7439, #15591, #17060, #14514, #6248 ),
 .UNSPECIFIED., .F., .T. ) 
 B_SPLINE_CURVE_WITH_KNOTS ( ( 3, 2, 2, 2, 3 ),
 ( 0.7115384615384615641, 0.7179487179487179516, 0.7307692307692307265, 0.7435897435897436125, 0.7500000000000000000 ),
 .UNSPECIFIED. ) 
 CURVE ( )  GEOMETRIC_REPRESENTATION_ITEM ( )  RATIONAL_B_SPLINE_CURVE ( ( 0.9330127018922194093, 0.9330127018922194093, 1.000000000000000000, 0.8660254037844387076, 1.000000000000000000, 0.8660254037844387076, 1.000000000000000000, 0.9330127018922194093, 0.9330127018922194093 ) ) 
 REPRESENTATION_ITEM ( '' )  );
#8781 = CARTESIAN_POINT ( 'NONE',  ( 33.40754056521197413, -5.892811586081919906, -6.861505862736166250 ) ) ;
#8782 = PLANE ( 'NONE',  #10667 ) ;
#8783 = DIRECTION ( 'NONE',  ( -0.000000000000000000, -0.000000000000000000, 1.000000000000000000 ) ) ;
#8784 = AXIS2_PLACEMENT_3D ( 'NONE', #10539, #9276, #7837 ) ;
#8785 = CARTESIAN_POINT ( 'NONE',  ( 32.65880277236253448, -4.102108105263264193, -7.939653947423662039 ) ) ;
#8786 = ORIENTED_EDGE ( 'NONE', *, *, #14794, .T. ) ;
#8787 = EDGE_CURVE ( 'NONE', #5290, #17723, #17601, .T. ) ;
#8788 = CARTESIAN_POINT ( 'NONE',  ( 19.71718888926881164, -28.93397812220195675, 15.64003640126281347 ) ) ;
#8789 = CARTESIAN_POINT ( 'NONE',  ( 32.14656953781143756, -4.163822094218565972, 8.283357778048662468 ) ) ;
#8790 = AXIS2_PLACEMENT_3D ( 'NONE', #14696, #11961, #11866 ) ;
#8791 = VERTEX_POINT ( 'NONE', #1645 ) ;
#8792 = ORIENTED_EDGE ( 'NONE', *, *, #17495, .F. ) ;
#8793 = ORIENTED_EDGE ( 'NONE', *, *, #2508, .F. ) ;
#8794 = DIRECTION ( 'NONE',  ( 0.9928203230275510771, 0.1196152422706609902, 4.006172263299092517E-17 ) ) ;
#8795 = CARTESIAN_POINT ( 'NONE',  ( 33.44685390376565692, -4.007163506710925027, 3.627061608673664228 ) ) ;
#8796 = FACE_BOUND ( 'NONE', #8024, .T. ) ;
#8797 = DIRECTION ( 'NONE',  ( -1.000000000000000000, 0.000000000000000000, 0.000000000000000000 ) ) ;
#8798 = EDGE_CURVE ( 'NONE', #16186, #5245, #7179, .T. ) ;
#8799 = PLANE ( 'NONE',  #621 ) ;
#8800 = CARTESIAN_POINT ( 'NONE',  ( 25.58373587974369201, -2.446631813008643075, -5.783357778048658027 ) ) ;
#8801 = CARTESIAN_POINT ( 'NONE',  ( 45.00000000000000711, -16.03270077640482683, 0.5379818257722508434 ) ) ;
#8802 = CARTESIAN_POINT ( 'NONE',  ( 29.35841309260160159, -6.680460261459264970, -4.533357778048668685 ) ) ;
#8803 = DIRECTION ( 'NONE',  ( -0.000000000000000000, -0.000000000000000000, -1.000000000000000000 ) ) ;
#8804 = PRODUCT_DEFINITION_CONTEXT ( 'detailed design', #2061, 'design' ) ;
#8805 = CARTESIAN_POINT ( 'NONE',  ( 26.02974819644417792, -2.720057890826728109, -4.533357778048659803 ) ) ;
#8806 = VERTEX_POINT ( 'NONE', #280 ) ;
#8807 = ORIENTED_EDGE ( 'NONE', *, *, #17630, .T. ) ;
#8808 = CARTESIAN_POINT ( 'NONE',  ( 26.87106449706838873, -6.053357334259913181, -3.627061608673667781 ) ) ;
#8809 = FACE_OUTER_BOUND ( 'NONE', #4590, .T. ) ;
#8810 = CARTESIAN_POINT ( 'NONE',  ( 14.00000000000000178, 1.714505518806294835E-15, -8.700000000000001066 ) ) ;
#8811 = CARTESIAN_POINT ( 'NONE',  ( 33.76207435632690590, -3.969185667289998332, -3.627061608673664672 ) ) ;
#8812 = CARTESIAN_POINT ( 'NONE',  ( 26.01652455409633902, -4.902371455920928156, -5.783357778048663356 ) ) ;
#8813 = CARTESIAN_POINT ( 'NONE',  ( 29.07687923786957285, -2.352938776424351008, 4.533357778048667797 ) ) ;
#8814 = DIRECTION ( 'NONE',  ( 1.000000000000000000, 0.000000000000000000, -0.000000000000000000 ) ) ;
#8815 = ORIENTED_EDGE ( 'NONE', *, *, #12160, .F. ) ;
#8816 = DIRECTION ( 'NONE',  ( -0.000000000000000000, -0.000000000000000000, -1.000000000000000000 ) ) ;
#8817 = EDGE_LOOP ( 'NONE', ( #8493, #11914 ) ) ;
#8818 = EDGE_CURVE ( 'NONE', #1659, #10101, #12122, .T. ) ;
#8819 = DIRECTION ( 'NONE',  ( 1.000000000000000000, 0.000000000000000000, 0.000000000000000000 ) ) ;
#8820 = DIRECTION ( 'NONE',  ( -1.000000000000000000, 0.000000000000000000, 0.000000000000000000 ) ) ;
#8821 = CARTESIAN_POINT ( 'NONE',  ( 27.00222791626931240, -2.275731535614434531, -5.783357778048658915 ) ) ;
#8822 = CARTESIAN_POINT ( 'NONE',  ( 26.86291784143654127, -6.981118157082444320, -7.033357778048666908 ) ) ;
#8823 = ORIENTED_EDGE ( 'NONE', *, *, #13686, .F. ) ;
#8824 = CARTESIAN_POINT ( 'NONE',  ( 26.98483462626008134, -4.785709214840094816, -7.939653947423662039 ) ) ;
#8825 = FACE_OUTER_BOUND ( 'NONE', #9055, .T. ) ;
#8826 = CARTESIAN_POINT ( 'NONE',  ( 28.45891156537951971, -2.090033060632186412, -5.783357778048670461 ) ) ;
#8827 = PLANE ( 'NONE',  #5420 ) ;
#8828 = CARTESIAN_POINT ( 'NONE',  ( 31.63243098167119172, -2.771952051906466874, -8.283357778048658915 ) ) ;
#8829 = CARTESIAN_POINT ( 'NONE',  ( 29.06119811526816576, -2.017469425591354337, -6.453230759126464378 ) ) ;
#8830 = CARTESIAN_POINT ( 'NONE',  ( 31.38469755857769528, -2.374701023479507178, 6.861505862736165362 ) ) ;
#8831 = DIRECTION ( 'NONE',  ( -0.5999999999999999778, -0.7999999999999999334, 0.000000000000000000 ) ) ;
#8832 = CARTESIAN_POINT ( 'NONE',  ( -35.41536221060850664, -16.03270077640482683, 0.5379818257722508434 ) ) ;
#8833 = CARTESIAN_POINT ( 'NONE',  ( 28.11132641904908169, -7.168068194032743534, 5.783357778048657138 ) ) ;
#8834 = ORIENTED_EDGE ( 'NONE', *, *, #13382, .F. ) ;
#8835 = CARTESIAN_POINT ( 'NONE',  ( 35.74085044863416982, -18.73429073671341172, -11.27079897466147251 ) ) ;
#8836 = ORIENTED_EDGE ( 'NONE', *, *, #13511, .T. ) ;
#8837 = CARTESIAN_POINT ( 'NONE',  ( 9.099998387031005720, -19.29508120620799971, -16.81964500401478091 ) ) ;
#8838 = EDGE_CURVE ( 'NONE', #13298, #2020, #17207, .T. ) ;
#8839 = DIRECTION ( 'NONE',  ( -0.7071067811865254793, 8.659560562355202797E-17, -0.7071067811865695552 ) ) ;
#8840 = CARTESIAN_POINT ( 'NONE',  ( 26.87785582392756112, -3.344784462964796035, -3.283357778048662023 ) ) ;
#8841 = CARTESIAN_POINT ( 'NONE',  ( 30.03006034954003667, -2.965006068755446478, -3.283357778048662023 ) ) ;
#8842 = CARTESIAN_POINT ( 'NONE',  ( 8.472608240843633681E-22, -7.722472891792491889E-22, -7.794427190999915211 ) ) ;
#8843 = CARTESIAN_POINT ( 'NONE',  ( 2.500000000000000000, 1.178949249685218081, 2.041999999999998483 ) ) ;
#8844 = EDGE_CURVE ( 'NONE', #15290, #6324, #6604, .T. ) ;
#8845 = CARTESIAN_POINT ( 'NONE',  ( 32.67619606237177265, -1.592130426037603907, -5.783357778048658027 ) ) ;
#8846 = CARTESIAN_POINT ( 'NONE',  ( 39.55500000000002103, 3.061616997868384127E-16, -2.500000000000000888 ) ) ;
#8847 = AXIS2_PLACEMENT_3D ( 'NONE', #6582, #9641, #16554 ) ;
#8848 = DIRECTION ( 'NONE',  ( 0.000000000000000000, -1.000000000000000000, 0.000000000000000000 ) ) ;
#8849 = CARTESIAN_POINT ( 'NONE',  ( 33.95908713831676096, -3.945449517755638791, 8.283357778048662468 ) ) ;
#8850 = ORIENTED_EDGE ( 'NONE', *, *, #4828, .F. ) ;
#8851 = B_SPLINE_CURVE_WITH_KNOTS ( 'NONE', 1,
 ( #16287, #14657 ),
 .UNSPECIFIED., .F., .F.,
 ( 2, 2 ),
 ( 0.000000000000000000, 1.000000000000000000 ),
 .UNSPECIFIED. ) ;
#8852 = DIRECTION ( 'NONE',  ( -0.05980762113533193841, 0.4964101615137754275, 0.8660254037844385966 ) ) ;
#8853 = VERTEX_POINT ( 'NONE', #2278 ) ;
#8854 = CARTESIAN_POINT ( 'NONE',  ( 26.34117031759772942, -2.982346454214467535, 6.861505862736165362 ) ) ;
#8855 = CARTESIAN_POINT ( 'NONE',  ( 26.01652455409633902, -4.902371455920928156, -5.783357778048663356 ) ) ;
#8856 = CARTESIAN_POINT ( 'NONE',  ( -2.682243648011669368, -3.070208061305314207, -0.04852650426602043987 ) ) ;
#8857 = ORIENTED_EDGE ( 'NONE', *, *, #6849, .F. ) ;
#8858 = CARTESIAN_POINT ( 'NONE',  ( 34.43754810739937966, -7.916730809865828888, -5.783357778048663356 ) ) ;
#8859 = ORIENTED_EDGE ( 'NONE', *, *, #13855, .T. ) ;
#8860 = LINE ( 'NONE', #11659, #290 ) ;
#8861 = EDGE_CURVE ( 'NONE', #4895, #11071, #17715, .T. ) ;
#8862 = ORIENTED_EDGE ( 'NONE', *, *, #6551, .T. ) ;
#8863 = CARTESIAN_POINT ( 'NONE',  ( -3.586207239825857747E-13, 4.796734841935103688, -3.421909803043224230 ) ) ;
#8864 = CARTESIAN_POINT ( 'NONE',  ( 32.70264286945147347, -5.350767304972614546, -3.627061608673668225 ) ) ;
#8865 = CARTESIAN_POINT ( 'NONE',  ( 33.40301380667672504, -2.758504307001591549, -3.627061608673662896 ) ) ;
#8866 = CARTESIAN_POINT ( 'NONE',  ( 27.95193767517966776, -20.05341752217977103, 13.73231903009881627 ) ) ;
#8867 = DIRECTION ( 'NONE',  ( 0.000000000000000000, 0.000000000000000000, 1.000000000000000000 ) ) ;
#8868 = ADVANCED_FACE ( 'NONE', ( #2194 ), #12136, .T. ) ;
#8869 = CARTESIAN_POINT ( 'NONE',  ( 27.50150540219088313, -5.977401655418042914, -3.627061608673667781 ) ) ;
#8870 = VERTEX_POINT ( 'NONE', #16239 ) ;
#8871 = CARTESIAN_POINT ( 'NONE',  ( 26.39370705969127684, -2.976016814310973313, -6.861505862736158257 ) ) ;
#8872 = CARTESIAN_POINT ( 'NONE',  ( 31.92138306490751987, -2.737139032229836122, 8.283357778048664244 ) ) ;
#8873 = EDGE_CURVE ( 'NONE', #12535, #8691, #8983, .T. ) ;
#8874 = ORIENTED_EDGE ( 'NONE', *, *, #2408, .T. ) ;
#8875 = VERTEX_POINT ( 'NONE', #10756 ) ;
#8876 =( BOUNDED_CURVE ( )  B_SPLINE_CURVE ( 2, ( #2386, #6803, #7903, #7812, #1095, #17895, #5249, #13341, #9422 ),
 .UNSPECIFIED., .F., .T. ) 
 B_SPLINE_CURVE_WITH_KNOTS ( ( 3, 2, 2, 2, 3 ),
 ( 0.6346153846153846922, 0.6410256410256410797, 0.6538461538461538547, 0.6666666666666666297, 0.6730769230769231282 ),
 .UNSPECIFIED. ) 
 CURVE ( )  GEOMETRIC_REPRESENTATION_ITEM ( )  RATIONAL_B_SPLINE_CURVE ( ( 0.9330127018922192983, 0.9330127018922198534, 1.000000000000000000, 0.8660254037844387076, 1.000000000000000000, 0.8660254037844387076, 1.000000000000000000, 0.9330127018922187432, 0.9330127018922192983 ) ) 
 REPRESENTATION_ITEM ( '' )  );
#8877 = ORIENTED_EDGE ( 'NONE', *, *, #5350, .F. ) ;
#8878 = CARTESIAN_POINT ( 'NONE',  ( -23.02601376483258022, 3.965314980223224151, 0.000000000000000000 ) ) ;
#8879 = CARTESIAN_POINT ( 'NONE',  ( -23.00000000000000000, -16.21813761408365195, -0.000000000000000000 ) ) ;
#8880 = CARTESIAN_POINT ( 'NONE',  ( 27.82847066025702887, -2.165988739474055791, -5.783357778048658027 ) ) ;
#8881 = CARTESIAN_POINT ( 'NONE',  ( 2.500000000000000000, 0.000000000000000000, -10.00000000000000000 ) ) ;
#8882 = ADVANCED_FACE ( 'NONE', ( #4883 ), #9912, .F. ) ;
#8883 = CARTESIAN_POINT ( 'NONE',  ( -27.94765010173961883, -20.05889348609997924, -13.73347386810006832 ) ) ;
#8884 = CARTESIAN_POINT ( 'NONE',  ( 32.70264286945147347, -5.350767304972614546, -3.627061608673668225 ) ) ;
#8885 = CARTESIAN_POINT ( 'NONE',  ( -2.500000000000000000, 3.061616997868383141E-16, -3.000000000000000000 ) ) ;
#8886 = DIRECTION ( 'NONE',  ( 0.000000000000000000, 0.000000000000000000, 1.000000000000000000 ) ) ;
#8887 = CARTESIAN_POINT ( 'NONE',  ( 28.63031693179632242, -2.406740715396564756, -4.533357778048659803 ) ) ;
#8888 = DIRECTION ( 'NONE',  ( -0.000000000000000000, -0.000000000000000000, 1.000000000000000000 ) ) ;
#8889 = CARTESIAN_POINT ( 'NONE',  ( 27.96989853965305528, -4.667028466753395222, -8.283357778048662468 ) ) ;
#8890 = VERTEX_POINT ( 'NONE', #3812 ) ;
#8891 = ORIENTED_EDGE ( 'NONE', *, *, #6355, .T. ) ;
#8892 = CARTESIAN_POINT ( 'NONE',  ( 27.51889869220010354, -3.467423976192371082, -7.939653947423660263 ) ) ;
#8893 = CARTESIAN_POINT ( 'NONE',  ( 40.00000000000000000, 2.055000000000000160, 0.000000000000000000 ) ) ;
#8894 = ORIENTED_EDGE ( 'NONE', *, *, #3157, .T. ) ;
#8895 = CARTESIAN_POINT ( 'NONE',  ( 0.000000000000000000, 0.000000000000000000, -3.000000000000000000 ) ) ;
#8896 = EDGE_CURVE ( 'NONE', #172, #4942, #5180, .T. ) ;
#8897 = CARTESIAN_POINT ( 'NONE',  ( 29.98133424373737910, -5.878503772023492502, 3.283357778048663800 ) ) ;
#8898 = AXIS2_PLACEMENT_3D ( 'NONE', #4024, #7204, #12449 ) ;
#8899 = ORIENTED_EDGE ( 'NONE', *, *, #6159, .T. ) ;
#8900 = CARTESIAN_POINT ( 'NONE',  ( 25.98779870451785001, -2.387753359738024272, 5.113484796970856117 ) ) ;
#8901 = CARTESIAN_POINT ( 'NONE',  ( 31.27962407439061110, -2.387360303286481855, -6.861505862736159145 ) ) ;
#8902 = ORIENTED_EDGE ( 'NONE', *, *, #12443, .F. ) ;
#8903 = ORIENTED_EDGE ( 'NONE', *, *, #4901, .F. ) ;
#8904 = CARTESIAN_POINT ( 'NONE',  ( 45.00000000000000711, -19.03270077640483038, -5.537981825772250843 ) ) ;
#8905 = CARTESIAN_POINT ( 'NONE',  ( 39.85968403307006014, -4.832501846690662184, -8.531230242176626177 ) ) ;
#8906 = VERTEX_POINT ( 'NONE', #1437 ) ;
#8907 = CARTESIAN_POINT ( 'NONE',  ( 27.45766530510195835, -4.728742455708699666, -3.627061608673664672 ) ) ;
#8908 = CARTESIAN_POINT ( 'NONE',  ( 26.19678349485696955, -4.880653813392439311, -3.627061608673664672 ) ) ;
#8909 = CIRCLE ( 'NONE', #2270, 2.500000000000001776 ) ;
#8910 = CARTESIAN_POINT ( 'NONE',  ( 28.38593337277646711, -7.124786616671554107, -5.783357778048668685 ) ) ;
#8911 = CARTESIAN_POINT ( 'NONE',  ( 1.746467850512308208E-21, -1.591841644184202181E-21, -6.005572809000082835 ) ) ;
#8912 = CARTESIAN_POINT ( 'NONE',  ( 31.34233605952372415, -6.778795339760710803, -5.783357778048663356 ) ) ;
#8913 = FACE_OUTER_BOUND ( 'NONE', #17912, .T. ) ;
#8914 = CARTESIAN_POINT ( 'NONE',  ( 29.38468146192651886, -6.677295441714964142, -7.033357778048666908 ) ) ;
#8915 = EDGE_CURVE ( 'NONE', #10032, #7736, #10220, .T. ) ;
#8916 = LINE ( 'NONE', #17189, #12954 ) ;
#8917 = CARTESIAN_POINT ( 'NONE',  ( 30.62726312072365431, -1.838986382273682718, 5.783357778048668685 ) ) ;
#8918 = ORIENTED_EDGE ( 'NONE', *, *, #2209, .F. ) ;
#8919 = CARTESIAN_POINT ( 'NONE',  ( -4.000000000000004441, 2.309401076758499816, -3.204269196027524913 ) ) ;
#8920 = DIRECTION ( 'NONE',  ( 5.026720092345836698E-22, -4.581671729415424240E-22, 1.000000000000000000 ) ) ;
#8921 = ORIENTED_EDGE ( 'NONE', *, *, #13725, .T. ) ;
#8922 = DIRECTION ( 'NONE',  ( 0.000000000000000000, 0.000000000000000000, 1.000000000000000000 ) ) ;
#8923 = CARTESIAN_POINT ( 'NONE',  ( 25.78902048130849067, -3.014061381488925218, -4.757751673912568258 ) ) ;
#8924 = FACE_OUTER_BOUND ( 'NONE', #14485, .T. ) ;
#8925 = CARTESIAN_POINT ( 'NONE',  ( 33.13353876934985465, -5.498725377814142057, 3.283357778048663356 ) ) ;
#8926 = CARTESIAN_POINT ( 'NONE',  ( 29.81991338116587542, -2.990324628369393611, -8.283357778048658915 ) ) ;
#8927 = DIRECTION ( 'NONE',  ( 0.000000000000000000, 0.000000000000000000, 1.000000000000000000 ) ) ;
#8928 = CONTEXT_DEPENDENT_SHAPE_REPRESENTATION ( #11278, #1150 ) ;
#8929 = CARTESIAN_POINT ( 'NONE',  ( -23.00000000000000000, -16.21813761408365195, -0.000000000000000000 ) ) ;
#8930 = CARTESIAN_POINT ( 'NONE',  ( 29.13014440709066832, -5.781182818409868140, -7.939653947423664704 ) ) ;
#8931 = AXIS2_PLACEMENT_3D ( 'NONE', #8141, #1261, #1527 ) ;
#8932 = CARTESIAN_POINT ( 'NONE',  ( -7.666200962222379900, -6.158133996769632468, -2.333128398347828369 ) ) ;
#8933 = VECTOR ( 'NONE', #13306, 1000.000000000000227 ) ;
#8934 = EDGE_CURVE ( 'NONE', #7391, #1468, #17741, .T. ) ;
#8935 = CARTESIAN_POINT ( 'NONE',  ( 25.96860978910007844, -6.167287525404733017, 4.026412830637841722 ) ) ;
#8936 = ADVANCED_FACE ( 'NONE', ( #6788 ), #5498, .T. ) ;
#8937 = EDGE_LOOP ( 'NONE', ( #16006, #17407, #13381, #17762 ) ) ;
#8938 = CARTESIAN_POINT ( 'NONE',  ( 25.72395281601508898, -4.937620572523835349, -7.939653947423662039 ) ) ;
#8939 = ORIENTED_EDGE ( 'NONE', *, *, #12774, .F. ) ;
#8940 = CARTESIAN_POINT ( 'NONE',  ( 32.50119254608192421, -4.121097024973739309, 7.939653947423662039 ) ) ;
#8941 = CARTESIAN_POINT ( 'NONE',  ( -28.41103551745680633, -13.06362195986656616, 13.60745115249024728 ) ) ;
#8942 = CARTESIAN_POINT ( 'NONE',  ( 41.91396146090167463, 0.4627762229654553972, -5.783357778048662468 ) ) ;
#8943 = ADVANCED_FACE ( 'NONE', ( #11021 ), #2622, .F. ) ;
#8944 = ORIENTED_EDGE ( 'NONE', *, *, #2539, .F. ) ;
#8945 = DIRECTION ( 'NONE',  ( -0.6174492339697512655, -0.7866107318554506067, 0.000000000000000000 ) ) ;
#8946 = AXIS2_PLACEMENT_3D ( 'NONE', #5168, #16434, #2647 ) ;
#8947 = DIRECTION ( 'NONE',  ( 0.000000000000000000, 0.5000000000000009992, 0.8660254037844380415 ) ) ;
#8948 = CARTESIAN_POINT ( 'NONE',  ( 26.31046454879147944, -7.342107353655505264, -6.247327665911178052 ) ) ;
#8949 = CARTESIAN_POINT ( 'NONE',  ( 32.93470988637010066, -5.949778345213319497, -6.861505862736167138 ) ) ;
#8950 = ORIENTED_EDGE ( 'NONE', *, *, #829, .T. ) ;
#8951 = CARTESIAN_POINT ( 'NONE',  ( 26.31128205117621022, -7.047579375861630524, -7.033357778048666908 ) ) ;
#8952 = CARTESIAN_POINT ( 'NONE',  ( 2.500000000000000000, 1.178949249685213863, -2.042000000000001148 ) ) ;
#8953 = CYLINDRICAL_SURFACE ( 'NONE', #8963, 2.749999999999992895 ) ;
#8954 = CARTESIAN_POINT ( 'NONE',  ( 26.23609683341064525, -2.995005734021441768, -6.861505862736159145 ) ) ;
#8955 = CARTESIAN_POINT ( 'NONE',  ( 33.12669930479518854, -6.563814807098823145, -5.113484796970860558 ) ) ;
#8956 = CARTESIAN_POINT ( 'NONE',  ( 32.41296236253129592, -1.951006642345344044, 7.033357778048666020 ) ) ;
#8957 = VECTOR ( 'NONE', #14315, 1000.000000000000114 ) ;
#8958 = EDGE_CURVE ( 'NONE', #10072, #13311, #9355, .T. ) ;
#8959 = VERTEX_POINT ( 'NONE', #15213 ) ;
#8960 = ORIENTED_EDGE ( 'NONE', *, *, #7640, .T. ) ;
#8961 = VERTEX_POINT ( 'NONE', #79 ) ;
#8962 = LINE ( 'NONE', #16140, #13543 ) ;
#8963 = AXIS2_PLACEMENT_3D ( 'NONE', #6415, #13215, #4951 ) ;
#8964 = CARTESIAN_POINT ( 'NONE',  ( 32.04575515724927470, -1.668086104879473730, 5.783357778048668685 ) ) ;
#8965 = EDGE_CURVE ( 'NONE', #17429, #2247, #1257, .T. ) ;
#8966 = LINE ( 'NONE', #7616, #8631 ) ;
#8967 = PLANE ( 'NONE',  #10677 ) ;
#8968 = CARTESIAN_POINT ( 'NONE',  ( -16.75000000000000000, -16.21813761408365195, -16.03574476417183448 ) ) ;
#8969 = CARTESIAN_POINT ( 'NONE',  ( 26.36761712467744090, -6.740983333149474177, -4.705209693361168455 ) ) ;
#8970 = CARTESIAN_POINT ( 'NONE',  ( 32.95080301609915097, -1.548848848676412260, -5.783357778048663356 ) ) ;
#8971 = DIRECTION ( 'NONE',  ( 0.9928203230275510771, 0.1196152422706609902, 4.006172263299092517E-17 ) ) ;
#8972 = AXIS2_PLACEMENT_3D ( 'NONE', #11034, #10856, #10941 ) ;
#8973 = CARTESIAN_POINT ( 'NONE',  ( 1.243649364574536075E-15, 4.862606272033089816, -3.445885042887437244 ) ) ;
#8974 = CARTESIAN_POINT ( 'NONE',  ( 26.87785582392756112, -3.344784462964796035, -3.283357778048662023 ) ) ;
#8975 = CARTESIAN_POINT ( 'NONE',  ( 16.96391960790757736, -14.58372395263535282, 16.00480323547922978 ) ) ;
#8976 = DIRECTION ( 'NONE',  ( 0.000000000000000000, 0.000000000000000000, 1.000000000000000000 ) ) ;
#8977 = ORIENTED_EDGE ( 'NONE', *, *, #4806, .T. ) ;
#8978 = ADVANCED_BREP_SHAPE_REPRESENTATION ( '', ( #11433, #3575 ), #3784 ) ;
#8979 = CARTESIAN_POINT ( 'NONE',  ( 27.71165237056504438, -5.952083095804076684, -7.939653947423664704 ) ) ;
#8980 = CARTESIAN_POINT ( 'NONE',  ( 32.28234893270314387, -5.401404424200516807, -7.939653947423662927 ) ) ;
#8981 = ORIENTED_EDGE ( 'NONE', *, *, #15378, .F. ) ;
#8982 = CIRCLE ( 'NONE', #6096, 3.999999999999994671 ) ;
#8983 =( BOUNDED_CURVE ( )  B_SPLINE_CURVE ( 2, ( #1082, #6342, #3635, #907, #9236, #7976, #7797, #17346, #810 ),
 .UNSPECIFIED., .F., .T. ) 
 B_SPLINE_CURVE_WITH_KNOTS ( ( 3, 2, 2, 2, 3 ),
 ( 0.4807692307692307820, 0.4871794871794871695, 0.5000000000000000000, 0.5128205128205127750, 0.5192307692307692735 ),
 .UNSPECIFIED. ) 
 CURVE ( )  GEOMETRIC_REPRESENTATION_ITEM ( )  RATIONAL_B_SPLINE_CURVE ( ( 0.9330127018922194093, 0.9330127018922196314, 1.000000000000000000, 0.8660254037844387076, 1.000000000000000000, 0.8660254037844387076, 1.000000000000000000, 0.9330127018922187432, 0.9330127018922192983 ) ) 
 REPRESENTATION_ITEM ( '' )  );
#8984 = DIRECTION ( 'NONE',  ( 0.000000000000000000, 0.000000000000000000, -1.000000000000000000 ) ) ;
#8985 = CARTESIAN_POINT ( 'NONE',  ( 28.72045243349238675, -6.030415129707233035, 3.283357778048663800 ) ) ;
#8986 = VECTOR ( 'NONE', #494, 1000.000000000000227 ) ;
#8987 = ORIENTED_EDGE ( 'NONE', *, *, #1850, .T. ) ;
#8988 = DIRECTION ( 'NONE',  ( -1.000000000000000000, 0.000000000000000000, 0.000000000000000000 ) ) ;
#8989 = CARTESIAN_POINT ( 'NONE',  ( 29.99682221560115991, -1.914942061115552541, -5.783357778048658915 ) ) ;
#8990 = ORIENTED_EDGE ( 'NONE', *, *, #17495, .T. ) ;
#8991 = DIRECTION ( 'NONE',  ( 0.000000000000000000, -1.000000000000000000, -0.000000000000000000 ) ) ;
#8992 = TOROIDAL_SURFACE ( 'NONE', #7841, 10.40000000000000036, 0.9000000000000003553 ) ;
#8993 = DIRECTION ( 'NONE',  ( -0.000000000000000000, -0.000000000000000000, -1.000000000000000000 ) ) ;
#8994 = AXIS2_PLACEMENT_3D ( 'NONE', #13104, #16016, #681 ) ;
#8995 = CARTESIAN_POINT ( 'NONE',  ( 0.5469803261931410754, -4.303002914948000246, -3.235259548910958127 ) ) ;
#8996 = EDGE_CURVE ( 'NONE', #3773, #8628, #2529, .T. ) ;
#8997 = CARTESIAN_POINT ( 'NONE',  ( 27.02414796481377124, -2.900061135469103490, -6.861505862736158257 ) ) ;
#8998 = VECTOR ( 'NONE', #10772, 1000.000000000000000 ) ;
#8999 = CARTESIAN_POINT ( 'NONE',  ( 25.62757597683262034, -3.695291012717980994, -7.939653947423660263 ) ) ;
#9000 = CARTESIAN_POINT ( 'NONE',  ( 28.13948077428293715, -7.164676150231702678, -6.453230759126474148 ) ) ;
#9001 = DIRECTION ( 'NONE',  ( 0.9928203230275510771, 0.1196152422706609902, 4.006172263299092517E-17 ) ) ;
#9002 = CARTESIAN_POINT ( 'NONE',  ( 26.79905070906540132, -3.354278923027479209, -3.283357778048662023 ) ) ;
#9003 =( BOUNDED_CURVE ( )  B_SPLINE_CURVE ( 2, ( #8757, #9909, #14288, #3310, #12728, #8840, #4660, #1682, #4567 ),
 .UNSPECIFIED., .F., .T. ) 
 B_SPLINE_CURVE_WITH_KNOTS ( ( 3, 2, 2, 2, 3 ),
 ( 0.7500000000000000000, 0.7564102564102563875, 0.7692307692307692735, 0.7820512820512820484, 0.7884615384615384359 ),
 .UNSPECIFIED. ) 
 CURVE ( )  GEOMETRIC_REPRESENTATION_ITEM ( )  RATIONAL_B_SPLINE_CURVE ( ( 0.9330127018922194093, 0.9330127018922194093, 1.000000000000000000, 0.8660254037844387076, 1.000000000000000000, 0.8660254037844387076, 1.000000000000000000, 0.9330127018922194093, 0.9330127018922194093 ) ) 
 REPRESENTATION_ITEM ( '' )  );
#9004 = FACE_OUTER_BOUND ( 'NONE', #13946, .T. ) ;
#9005 = CONICAL_SURFACE ( 'NONE', #1192, 9.500000000000001776, 0.7853981633974465026 ) ;
#9006 = AXIS2_PLACEMENT_3D ( 'NONE', #3353, #807, #15965 ) ;
#9007 = VERTEX_POINT ( 'NONE', #16674 ) ;
#9008 = DIRECTION ( 'NONE',  ( 0.9928203230275512992, 0.1196152422706610180, 4.006172263299093133E-17 ) ) ;
#9009 = DIRECTION ( 'NONE',  ( 0.000000000000000000, 0.000000000000000000, 1.000000000000000000 ) ) ;
#9010 = DIRECTION ( 'NONE',  ( 0.9928203230275512992, 0.1196152422706610180, 4.006172263299093133E-17 ) ) ;
#9011 = ORIENTED_EDGE ( 'NONE', *, *, #8554, .T. ) ;
#9012 = CARTESIAN_POINT ( 'NONE',  ( -3.538288549924106796, -15.34800872113743431, 16.99955934415556769 ) ) ;
#9013 = DIRECTION ( 'NONE',  ( -0.000000000000000000, -1.000000000000000000, -0.000000000000000000 ) ) ;
#9014 = CARTESIAN_POINT ( 'NONE',  ( -9.166200962222282200, 3.560057785416494980, -2.333128398347827037 ) ) ;
#9015 = CARTESIAN_POINT ( 'NONE',  ( 32.08959525433819238, -2.916745304588811205, -7.939653947423660263 ) ) ;
#9016 = EDGE_CURVE ( 'NONE', #10739, #8961, #4248, .T. ) ;
#9017 = CARTESIAN_POINT ( 'NONE',  ( 33.16732689266149237, -6.221561368663743430, 4.533357778048659803 ) ) ;
#9018 = CIRCLE ( 'NONE', #1496, 5.500000000000000000 ) ;
#9019 = ADVANCED_FACE ( 'NONE', ( #8409 ), #8056, .T. ) ;
#9020 = AXIS2_PLACEMENT_3D ( 'NONE', #12423, #4186, #9687 ) ;
#9021 = CARTESIAN_POINT ( 'NONE',  ( 28.20260476654369697, -6.819712339336020612, -7.033357778048666908 ) ) ;
#9022 = CARTESIAN_POINT ( 'NONE',  ( -1.391697335622809950, -4.043246145443384343, -3.203898532754370532 ) ) ;
#9023 = DIRECTION ( 'NONE',  ( -0.1196152422706610735, 0.9928203230275511881, 0.000000000000000000 ) ) ;
#9024 = CARTESIAN_POINT ( 'NONE',  ( 28.51709679197739078, -3.347160818026084339, -3.627061608673662008 ) ) ;
#9025 = DIRECTION ( 'NONE',  ( 0.1113444980252557837, 0.9937818688019538493, -0.000000000000000000 ) ) ;
#9026 = CARTESIAN_POINT ( 'NONE',  ( 25.74134610602432360, -2.427642893298174620, 5.783357778048668685 ) ) ;
#9027 = ORIENTED_EDGE ( 'NONE', *, *, #17198, .F. ) ;
#9028 = AXIS2_PLACEMENT_3D ( 'NONE', #10018, #13185, #9105 ) ;
#9029 = VERTEX_POINT ( 'NONE', #13594 ) ;
#9030 = AXIS2_PLACEMENT_3D ( 'NONE', #13971, #8082, #13617 ) ;
#9031 = CARTESIAN_POINT ( 'NONE',  ( 26.23609683341064525, -2.995005734021441768, -6.861505862736159145 ) ) ;
#9032 = ORIENTED_EDGE ( 'NONE', *, *, #7265, .T. ) ;
#9033 = CARTESIAN_POINT ( 'NONE',  ( 33.33308377457396432, -5.274811626130743392, 7.939653947423658487 ) ) ;
#9034 = CARTESIAN_POINT ( 'NONE',  ( 29.37220822929407760, -7.016156836349003001, -5.783357778048668685 ) ) ;
#9035 = CARTESIAN_POINT ( 'NONE',  ( 27.49335874655903567, -6.905162478240574053, -7.033357778048666908 ) ) ;
#9036 = ORIENTED_EDGE ( 'NONE', *, *, #15758, .F. ) ;
#9037 = DIRECTION ( 'NONE',  ( 0.000000000000000000, 0.000000000000000000, -1.000000000000000000 ) ) ;
#9038 = TOROIDAL_SURFACE ( 'NONE', #16551, 5.384454397937117776, 0.5155456020628805813 ) ;
#9039 = CARTESIAN_POINT ( 'NONE',  ( 2.500000000000000000, 2.357898499370432166, -2.385244779468109755E-15 ) ) ;
#9040 = DIRECTION ( 'NONE',  ( -0.1196152422706621143, -0.9928203230275509661, -0.000000000000000000 ) ) ;
#9041 = CARTESIAN_POINT ( 'NONE',  ( -4.000000000000000000, 2.309401076758501592, -3.133295621305381307 ) ) ;
#9042 = CARTESIAN_POINT ( 'NONE',  ( 32.14665875496697822, -6.044722943765660439, -6.861505862736166250 ) ) ;
#9043 = CARTESIAN_POINT ( 'NONE',  ( 31.03132594549780876, -1.780107929003061473, 5.113484796970860558 ) ) ;
#9044 = FACE_OUTER_BOUND ( 'NONE', #13038, .T. ) ;
#9045 = PRESENTATION_STYLE_ASSIGNMENT (( #10390 ) ) ;
#9046 = CARTESIAN_POINT ( 'NONE',  ( 28.73594040535616756, -2.066853418799292630, -5.783357778048658027 ) ) ;
#9047 = VECTOR ( 'NONE', #13798, 1000.000000000000227 ) ;
#9048 = ADVANCED_FACE ( 'NONE', ( #11386 ), #1712, .T. ) ;
#9049 = DIRECTION ( 'NONE',  ( -5.026720092345836698E-22, 4.581671729415424240E-22, -1.000000000000000000 ) ) ;
#9050 = VECTOR ( 'NONE', #9917, 1000.000000000000000 ) ;
#9051 = CARTESIAN_POINT ( 'NONE',  ( 30.52163964716380917, -2.178873678870954400, 7.033357778048666020 ) ) ;
#9052 = AXIS2_PLACEMENT_3D ( 'NONE', #10924, #17801, #5321 ) ;
#9053 = ORIENTED_EDGE ( 'NONE', *, *, #12117, .F. ) ;
#9054 = ORIENTED_EDGE ( 'NONE', *, *, #9088, .T. ) ;
#9055 = EDGE_LOOP ( 'NONE', ( #14830, #12593, #14899, #11421 ) ) ;
#9056 = CARTESIAN_POINT ( 'NONE',  ( 4.000000000000000000, 2.309401076758498483, -4.700000000000000178 ) ) ;
#9057 = CARTESIAN_POINT ( 'NONE',  ( 32.80318959510331212, -2.203800746085299522, 6.861505862736166250 ) ) ;
#9058 = VERTEX_POINT ( 'NONE', #8689 ) ;
#9059 = CARTESIAN_POINT ( 'NONE',  ( 45.50000000000000000, -16.03270077640482683, 5.537981825772250843 ) ) ;
#9060 = VECTOR ( 'NONE', #14836, 1000.000000000000227 ) ;
#9061 = CARTESIAN_POINT ( 'NONE',  ( -28.29220412912503946, -19.54937045720491184, -13.63977809545137454 ) ) ;
#9062 = CARTESIAN_POINT ( 'NONE',  ( 30.82871344409320713, -3.068656662272551738, -7.939653947423660263 ) ) ;
#9063 = CARTESIAN_POINT ( 'NONE',  ( 10.89999065189540772, 4.519978295146206193, -9.600000000000001421 ) ) ;
#9064 = PLANE ( 'NONE',  #7272 ) ;
#9065 = CIRCLE ( 'NONE', #3569, 3.999999999999999112 ) ;
#9066 = TOROIDAL_SURFACE ( 'NONE', #1843, 10.40000000000000036, 0.9000000000000003553 ) ;
#9068 = EDGE_CURVE ( 'NONE', #2513, #15456, #4724, .T. ) ;
#9067 = CARTESIAN_POINT ( 'NONE',  ( 2.500000000000000000, 0.000000000000000000, 0.000000000000000000 ) ) ;
#9069 = CARTESIAN_POINT ( 'NONE',  ( 27.10304229683147526, -4.771467524953526329, -3.283357778048664688 ) ) ;
#9070 = CARTESIAN_POINT ( 'NONE',  ( -18.96667930129623514, 9.308258642545592210, 15.69246997591053017 ) ) ;
#9071 = SHAPE_REPRESENTATION_RELATIONSHIP ( 'NONE' , 'NONE' ,  #16332, #8978 ) ;
#9072 = EDGE_LOOP ( 'NONE', ( #14852, #8698, #2355, #9269 ) ) ;
#9073 = CARTESIAN_POINT ( 'NONE',  ( 26.25801688195511474, -3.619335333876111171, -7.939653947423660263 ) ) ;
#9074 = AXIS2_PLACEMENT_3D ( 'NONE', #16413, #16492, #11189 ) ;
#9075 = CARTESIAN_POINT ( 'NONE',  ( 33.35047706458318828, -2.764833946905070672, -7.939653947423660263 ) ) ;
#9076 = EDGE_LOOP ( 'NONE', ( #1576, #8007, #3330, #5196 ) ) ;
#9077 = EDGE_CURVE ( 'NONE', #4496, #12037, #4596, .T. ) ;
#9078 = CARTESIAN_POINT ( 'NONE',  ( 25.93714794488954212, -2.393855775999666591, 5.783357778048667797 ) ) ;
#9079 = CARTESIAN_POINT ( 'NONE',  ( 25.95846283556873502, -3.455553161483296609, 3.283357778048666464 ) ) ;
#9080 = AXIS2_PLACEMENT_3D ( 'NONE', #11579, #14507, #10306 ) ;
#9081 = ORIENTED_EDGE ( 'NONE', *, *, #1252, .F. ) ;
#9082 = CARTESIAN_POINT ( 'NONE',  ( 32.55182397003001427, -2.661183353387966299, -3.283357778048662023 ) ) ;
#9083 = CARTESIAN_POINT ( 'NONE',  ( 32.02836186724004364, -4.178063784105134459, -7.939653947423662039 ) ) ;
#9084 = ORIENTED_EDGE ( 'NONE', *, *, #12401, .T. ) ;
#9085 = CARTESIAN_POINT ( 'NONE',  ( 29.14000323013032556, -2.007974965528672495, -6.453230759126468818 ) ) ;
#9086 = CARTESIAN_POINT ( 'NONE',  ( 33.47428445112562656, -1.485779673698264913, -6.453230759126466154 ) ) ;
#9087 = EDGE_LOOP ( 'NONE', ( #16301, #12192, #12592, #11143 ) ) ;
#9088 = EDGE_CURVE ( 'NONE', #11785, #8791, #12542, .T. ) ;
#9089 = CARTESIAN_POINT ( 'NONE',  ( -4.000000000000000000, -2.309401076758508253, -3.133295621305383083 ) ) ;
#9090 = CARTESIAN_POINT ( 'NONE',  ( 32.06776442294927421, -4.173316554281249147, -3.283357778048664688 ) ) ;
#9091 = CARTESIAN_POINT ( 'NONE',  ( 28.24571643650507369, -4.633797857156355171, -7.939653947423662039 ) ) ;
#9092 = DIRECTION ( 'NONE',  ( -0.8243186046180107640, 0.5661261679878573094, 0.000000000000000000 ) ) ;
#9093 = CARTESIAN_POINT ( 'NONE',  ( 32.85952466860454280, -1.897204703373130741, -7.033357778048658027 ) ) ;
#9094 = CARTESIAN_POINT ( 'NONE',  ( 4.906836669863238853, 17.52808241874658890, -16.98904569177533119 ) ) ;
#9095 = CARTESIAN_POINT ( 'NONE',  ( 29.91004888286193619, -6.613999042680076990, -4.533357778048668685 ) ) ;
#9096 = CARTESIAN_POINT ( 'NONE',  ( 31.08270050955629671, -4.291997302367946077, -3.627061608673664672 ) ) ;
#9097 = ADVANCED_FACE ( 'NONE', ( #15763 ), #15436, .T. ) ;
#9098 = EDGE_LOOP ( 'NONE', ( #5617, #5467, #1380, #2604 ) ) ;
#9099 = DIRECTION ( 'NONE',  ( -1.000000000000000000, -0.000000000000000000, -0.000000000000000000 ) ) ;
#9100 = CARTESIAN_POINT ( 'NONE',  ( 30.03006034954003667, -2.965006068755446478, -3.283357778048662023 ) ) ;
#9101 = LINE ( 'NONE', #14642, #3473 ) ;
#9102 = ORIENTED_EDGE ( 'NONE', *, *, #7589, .F. ) ;
#9103 = CARTESIAN_POINT ( 'NONE',  ( 25.90419076669538967, -3.969988049114257400, 3.653240910513405382 ) ) ;
#9104 = PRODUCT ( 'MirrorCaliper Body Half', 'MirrorCaliper Body Half', '', ( #1783 ) ) ;
#9105 = DIRECTION ( 'NONE',  ( 0.000000000000000000, 0.000000000000000000, -1.000000000000000000 ) ) ;
#9106 = CARTESIAN_POINT ( 'NONE',  ( -9.458171371210985612, 3.728626979641533001, -2.666481567098319072 ) ) ;
#9107 = CARTESIAN_POINT ( 'NONE',  ( 32.28234893270314387, -5.401404424200516807, -7.939653947423662927 ) ) ;
#9108 = CARTESIAN_POINT ( 'NONE',  ( 32.89331279191618762, -2.620040694222726785, 3.283357778048666464 ) ) ;
#9109 = EDGE_CURVE ( 'NONE', #1421, #15452, #1849, .T. ) ;
#9110 =( BOUNDED_CURVE ( )  B_SPLINE_CURVE ( 2, ( #425, #4401, #7134, #14103, #9916, #8665, #595, #8764, #3222 ),
 .UNSPECIFIED., .F., .T. ) 
 B_SPLINE_CURVE_WITH_KNOTS ( ( 3, 2, 2, 2, 3 ),
 ( 0.01923076923076924571, 0.02564102564102564014, 0.03846153846153846367, 0.05128205128205128027, 0.05769230769230770939 ),
 .UNSPECIFIED. ) 
 CURVE ( )  GEOMETRIC_REPRESENTATION_ITEM ( )  RATIONAL_B_SPLINE_CURVE ( ( 0.9330127018922194093, 0.9330127018922195203, 1.000000000000000000, 0.8660254037844387076, 1.000000000000000000, 0.8660254037844387076, 1.000000000000000000, 0.9330127018922191873, 0.9330127018922194093 ) ) 
 REPRESENTATION_ITEM ( '' )  );
#9111 = CARTESIAN_POINT ( 'NONE',  ( 27.26436163736424945, -2.571311352887278190, -7.033357778048658027 ) ) ;
#9112 = CARTESIAN_POINT ( 'NONE',  ( -15.92260893619738837, -28.39189527176317540, 12.00000000000000000 ) ) ;
#9113 = ITEM_DEFINED_TRANSFORMATION ( 'NONE', 'NONE', #4504,  #3575 ) ;
#9114 = LINE ( 'NONE', #10459, #4606 ) ;
#9115 = DIRECTION ( 'NONE',  ( -0.1196152422706610735, 0.9928203230275511881, 0.000000000000000000 ) ) ;
#9116 = CARTESIAN_POINT ( 'NONE',  ( 31.06530721954707985, -6.801974981593605030, -5.783357778048669573 ) ) ;
#9117 = DIRECTION ( 'NONE',  ( 1.000000000000000000, 0.000000000000000000, 0.000000000000000000 ) ) ;
#9118 = CARTESIAN_POINT ( 'NONE',  ( 29.47916769939009285, -7.003270332485284300, 5.113484796970857005 ) ) ;
#9119 = CARTESIAN_POINT ( 'NONE',  ( 28.49970350196817392, -5.857138497251738407, 3.627061608673662896 ) ) ;
#9120 = EDGE_CURVE ( 'NONE', #1819, #16114, #17675, .T. ) ;
#9121 = ORIENTED_EDGE ( 'NONE', *, *, #2301, .T. ) ;
#9122 = LINE ( 'NONE', #17833, #9890 ) ;
#9123 = VERTEX_POINT ( 'NONE', #1898 ) ;
#9124 = CARTESIAN_POINT ( 'NONE',  ( 25.71072941247523502, -3.058302133056337357, 6.861505862736165362 ) ) ;
#9125 = CARTESIAN_POINT ( 'NONE',  ( 27.27683486999669427, -2.232449958253242883, 5.783357778048667797 ) ) ;
#9126 = DIRECTION ( 'NONE',  ( 0.000000000000000000, 0.000000000000000000, 1.000000000000000000 ) ) ;
#9127 = VERTEX_POINT ( 'NONE', #2982 ) ;
#9128 = CARTESIAN_POINT ( 'NONE',  ( 28.71361296893772774, -7.095504558991913235, -5.113484796970856117 ) ) ;
#9129 = DIRECTION ( 'NONE',  ( 0.000000000000000000, 0.000000000000000000, -1.000000000000000000 ) ) ;
#9130 = DIRECTION ( 'NONE',  ( 0.1196152422706596996, -0.9928203230275514102, 0.000000000000000000 ) ) ;
#9131 = CARTESIAN_POINT ( 'NONE',  ( 32.91278983782564183, -5.325448745358647429, -7.939653947423664704 ) ) ;
#9132 = PRODUCT_RELATED_PRODUCT_CATEGORY ( 'part', '', ( #13304 ) ) ;
#9133 = CARTESIAN_POINT ( 'NONE',  ( 31.27962407439061110, -2.387360303286481855, -6.861505862736159145 ) ) ;
#9134 = MECHANICAL_DESIGN_GEOMETRIC_PRESENTATION_REPRESENTATION (  '', ( #6229 ), #5913 ) ;
#9135 = CARTESIAN_POINT ( 'NONE',  ( 31.08079519141086067, -2.838413270685653078, 3.283357778048666464 ) ) ;
#9136 = CARTESIAN_POINT ( 'NONE',  ( 26.31556265977298992, -7.384422263489805793, -5.783357778048663356 ) ) ;
#9137 = CARTESIAN_POINT ( 'NONE',  ( 29.41022140756759029, -3.239556939666760726, -7.939653947423660263 ) ) ;
#9138 = CARTESIAN_POINT ( 'NONE',  ( 33.20550441965735899, -6.554320347036139971, -5.113484796970860558 ) ) ;
#9139 = LINE ( 'NONE', #16890, #12983 ) ;
#9140 = CARTESIAN_POINT ( 'NONE',  ( 35.41536221060850664, -16.03270077640482683, -0.5379818257722508434 ) ) ;
#9141 = CARTESIAN_POINT ( 'NONE',  ( 31.04700706809921940, -2.115577279836057922, 4.533357778048667797 ) ) ;
#9142 = EDGE_CURVE ( 'NONE', #3354, #7716, #9790, .T. ) ;
#9143 = VERTEX_POINT ( 'NONE', #446 ) ;
#9144 = VERTEX_POINT ( 'NONE', #14316 ) ;
#9145 = ORIENTED_EDGE ( 'NONE', *, *, #10273, .F. ) ;
#9146 = ORIENTED_EDGE ( 'NONE', *, *, #6355, .F. ) ;
#9147 = CARTESIAN_POINT ( 'NONE',  ( 33.27602027394517847, -2.146833986953896822, 6.861505862736165362 ) ) ;
#9148 = CARTESIAN_POINT ( 'NONE',  ( 32.32618902979206865, -6.650063623909865385, 5.783357778048657138 ) ) ;
#9149 = ORIENTED_EDGE ( 'NONE', *, *, #11753, .T. ) ;
#9150 = DIRECTION ( 'NONE',  ( -0.9928203230275510771, -0.1196152422706614760, -0.000000000000000000 ) ) ;
#9151 = DIRECTION ( 'NONE',  ( -1.000000000000000000, 0.000000000000000000, 0.000000000000000000 ) ) ;
#9152 = CARTESIAN_POINT ( 'NONE',  ( 28.54354359905709870, -7.105797696961086096, -5.783357778048669573 ) ) ;
#9153 = CARTESIAN_POINT ( 'NONE',  ( 30.63309003953906995, -6.864245478665264244, -5.783357778048663356 ) ) ;
#9154 = EDGE_CURVE ( 'NONE', #4193, #10223, #5405, .T. ) ;
#9155 = DIRECTION ( 'NONE',  ( 0.000000000000000000, 0.000000000000000000, -1.000000000000000000 ) ) ;
#9156 = DIRECTION ( 'NONE',  ( 1.000000000000000000, 0.000000000000000000, 0.000000000000000000 ) ) ;
#9157 = CYLINDRICAL_SURFACE ( 'NONE', #16883, 95.00000000000000000 ) ;
#9158 = PRODUCT_DEFINITION_CONTEXT ( 'detailed design', #5728, 'design' ) ;
#9159 = CARTESIAN_POINT ( 'NONE',  ( 2.500000000000000000, 2.357898499370432166, -2.385244779468109755E-15 ) ) ;
#9160 = CARTESIAN_POINT ( 'NONE',  ( 32.93018312783485158, -2.815471066132994249, -3.627061608673662008 ) ) ;
#9161 = CARTESIAN_POINT ( 'NONE',  ( 30.82871344409320713, -3.068656662272551294, -7.939653947423660263 ) ) ;
#9162 = ORIENTED_EDGE ( 'NONE', *, *, #3910, .F. ) ;
#9163 = CARTESIAN_POINT ( 'NONE',  ( 5.560781378645575757, 0.000000000000000000, -3.700000000000000178 ) ) ;
#9164 = CARTESIAN_POINT ( 'NONE',  ( 26.89670596474818609, -7.703954147932045693, 5.783357778048657138 ) ) ;
#9165 = EDGE_CURVE ( 'NONE', #9649, #11134, #619, .T. ) ;
#9166 = ORIENTED_EDGE ( 'NONE', *, *, #4667, .F. ) ;
#9167 = CARTESIAN_POINT ( 'NONE',  ( 30.64918316926811315, -2.463315982128351678, -6.861505862736159145 ) ) ;
#9168 = ORIENTED_EDGE ( 'NONE', *, *, #11480, .T. ) ;
#9169 = CARTESIAN_POINT ( 'NONE',  ( 11.73134587110777005, 4.864722402403120149, -9.600000000000001421 ) ) ;
#9170 = CARTESIAN_POINT ( 'NONE',  ( -34.91600907648203389, -11.88801210197604341, -0.000000000000000000 ) ) ;
#9171 = DIRECTION ( 'NONE',  ( -0.1196152422706610735, 0.9928203230275511881, 0.000000000000000000 ) ) ;
#9172 = UNCERTAINTY_MEASURE_WITH_UNIT (LENGTH_MEASURE( 1.000000000000000082E-05 ), #6254, 'distance_accuracy_value', 'NONE');
#9173 = CARTESIAN_POINT ( 'NONE',  ( 31.07327543742414022, -2.112412460091767308, -4.533357778048659803 ) ) ;
#9174 = CARTESIAN_POINT ( 'NONE',  ( 27.75549246765397271, -7.200742295513423485, -5.783357778048668685 ) ) ;
#9175 = CARTESIAN_POINT ( 'NONE',  ( 27.19802975513453092, -2.241944418315925613, -5.783357778048658027 ) ) ;
#9176 = CARTESIAN_POINT ( 'NONE',  ( 30.64556327217151122, -6.525384084031224496, -7.033357778048666908 ) ) ;
#9177 = DIRECTION ( 'NONE',  ( -0.000000000000000000, -0.000000000000000000, -1.000000000000000000 ) ) ;
#9178 = CARTESIAN_POINT ( 'NONE',  ( 28.12379965168153362, -6.829206799398704675, -7.033357778048666908 ) ) ;
#9179 = CARTESIAN_POINT ( 'NONE',  ( 32.04158527077989760, -6.057382223572642665, -4.705209693361168455 ) ) ;
#9180 = EDGE_CURVE ( 'NONE', #17078, #15184, #7507, .T. ) ;
#9181 = EDGE_CURVE ( 'NONE', #364, #2020, #13268, .T. ) ;
#9182 = DIRECTION ( 'NONE',  ( -0.000000000000000000, 1.000000000000000000, -0.000000000000000000 ) ) ;
#9183 = CARTESIAN_POINT ( 'NONE',  ( 32.96626681528915981, -4.065064760026301016, 5.783357778048663356 ) ) ;
#9184 = EDGE_CURVE ( 'NONE', #7076, #12891, #6641, .T. ) ;
#9185 = ORIENTED_EDGE ( 'NONE', *, *, #17282, .F. ) ;
#9186 =( BOUNDED_CURVE ( )  B_SPLINE_CURVE ( 2, ( #10714, #14990, #5193, #6565, #2239, #12085, #862 ),
 .UNSPECIFIED., .F., .T. ) 
 B_SPLINE_CURVE_WITH_KNOTS ( ( 3, 2, 2, 3 ),
 ( 0.9423076923076922906, 0.9487179487179486781, 0.9615384615384615641, 0.9690340935984054216 ),
 .UNSPECIFIED. ) 
 CURVE ( )  GEOMETRIC_REPRESENTATION_ITEM ( )  RATIONAL_B_SPLINE_CURVE ( ( 0.9330127018922194093, 0.9330127018922194093, 1.000000000000000000, 0.8660254037844387076, 1.000000000000000000, 0.9216705062683109295, 0.9349331465915117212 ) ) 
 REPRESENTATION_ITEM ( '' )  );
#9187 = CARTESIAN_POINT ( 'NONE',  ( -35.41536221060850664, -16.03270077640482683, -10.53798182577225084 ) ) ;
#9188 = TOROIDAL_SURFACE ( 'NONE', #8015, 4.000000000000000000, 0.2500000000000000000 ) ;
#9189 = CARTESIAN_POINT ( 'NONE',  ( 33.56515079149260572, -5.873822666371450119, -6.861505862736167138 ) ) ;
#9190 = DIRECTION ( 'NONE',  ( 0.000000000000000000, 1.000000000000000000, 0.000000000000000000 ) ) ;
#9191 = EDGE_CURVE ( 'NONE', #5051, #4413, #16760, .T. ) ;
#9192 = CARTESIAN_POINT ( 'NONE',  ( 27.29814976067589072, -3.294147343736873346, -8.283357778048658915 ) ) ;
#9193 = DIRECTION ( 'NONE',  ( -0.1196152422706611151, 0.9928203230275511881, 0.000000000000000000 ) ) ;
#9194 = CARTESIAN_POINT ( 'NONE',  ( 27.48088551392658729, -7.244023872874614689, -5.783357778048657138 ) ) ;
#9195 = FACE_OUTER_BOUND ( 'NONE', #9995, .T. ) ;
#9196 = CARTESIAN_POINT ( 'NONE',  ( 30.29464937815318493, -4.386941900920275472, -7.939653947423662039 ) ) ;
#9197 = CARTESIAN_POINT ( 'NONE',  ( 28.82057243903374655, -7.082618055128190093, -5.783357778048668685 ) ) ;
#9198 = CARTESIAN_POINT ( 'NONE',  ( 33.73390066541284682, -2.518766455766908940, 8.283357778048666020 ) ) ;
#9199 = CARTESIAN_POINT ( 'NONE',  ( 28.30694982360322953, -3.372479377640031473, 3.627061608673666893 ) ) ;
#9200 = CIRCLE ( 'NONE', #6878, 2.055000000000000160 ) ;
#9201 = ORIENTED_EDGE ( 'NONE', *, *, #14410, .F. ) ;
#9202 = CARTESIAN_POINT ( 'NONE',  ( 31.06530721954707985, -6.801974981593605030, 5.783357778048657138 ) ) ;
#9203 = CARTESIAN_POINT ( 'NONE',  ( -28.84390385427241199, -13.99246034770667713, 13.48718205731130304 ) ) ;
#9204 = PLANE ( 'NONE',  #3857 ) ;
#9205 = VERTEX_POINT ( 'NONE', #17137 ) ;
#9206 = DIRECTION ( 'NONE',  ( 0.000000000000000000, 0.000000000000000000, -1.000000000000000000 ) ) ;
#9207 = LINE ( 'NONE', #14754, #8389 ) ;
#9208 = VERTEX_POINT ( 'NONE', #3152 ) ;
#9209 = CARTESIAN_POINT ( 'NONE',  ( 26.01652455409633902, -4.902371455920936150, 5.783357778048662468 ) ) ;
#9210 = CARTESIAN_POINT ( 'NONE',  ( 32.07220196432897552, -5.426722983814484813, -3.627061608673668225 ) ) ;
#9211 = CARTESIAN_POINT ( 'NONE',  ( 32.14213199643172914, -2.910415664685331638, -3.627061608673662896 ) ) ;
#9212 = EDGE_CURVE ( 'NONE', #10101, #15493, #7340, .T. ) ;
#9213 = CARTESIAN_POINT ( 'NONE',  ( -45.50000000000000000, -16.03270077640482683, -5.537981825772250843 ) ) ;
#9214 = CIRCLE ( 'NONE', #17370, 2.749999999999995559 ) ;
#9215 = CARTESIAN_POINT ( 'NONE',  ( 32.00093131988006689, -6.699447617117800569, -6.453230759126470595 ) ) ;
#9216 =( LENGTH_UNIT ( ) NAMED_UNIT ( * ) SI_UNIT ( .MILLI., .METRE. ) );
#9217 = CARTESIAN_POINT ( 'NONE',  ( 27.60205212784272177, -2.830435096530727446, -4.705209693361161349 ) ) ;
#9218 = DIRECTION ( 'NONE',  ( 0.000000000000000000, 0.000000000000000000, -1.000000000000000000 ) ) ;
#9219 = DIRECTION ( 'NONE',  ( 1.000000000000000000, 0.000000000000000000, 0.000000000000000000 ) ) ;
#9220 = CARTESIAN_POINT ( 'NONE',  ( 27.95866967485789090, -6.122194908100387245, 8.283357778048658915 ) ) ;
#9221 = ORIENTED_EDGE ( 'NONE', *, *, #16269, .T. ) ;
#9222 = ORIENTED_EDGE ( 'NONE', *, *, #9964, .T. ) ;
#9223 = AXIS2_PLACEMENT_3D ( 'NONE', #2705, #12389, #11010 ) ;
#9224 = ORIENTED_EDGE ( 'NONE', *, *, #1662, .T. ) ;
#9225 = CARTESIAN_POINT ( 'NONE',  ( 31.51621784984448738, -6.120678622607529817, 4.705209693361160461 ) ) ;
#9226 = CARTESIAN_POINT ( 'NONE',  ( 29.03376756790819613, -4.538853258604016006, 3.627061608673664228 ) ) ;
#9227 = ORIENTED_EDGE ( 'NONE', *, *, #13686, .T. ) ;
#9228 = CARTESIAN_POINT ( 'NONE',  ( -19.43845002722867221, 2.988003976273734263, -6.000000000000000000 ) ) ;
#9229 = DIRECTION ( 'NONE',  ( 1.000000000000000000, 0.000000000000000000, 0.000000000000000000 ) ) ;
#9230 = CARTESIAN_POINT ( 'NONE',  ( 30.29464937815318493, -4.386941900920275472, -7.939653947423662039 ) ) ;
#9231 = CARTESIAN_POINT ( 'NONE',  ( 29.06119811526816576, -2.017469425591354337, 5.113484796970861446 ) ) ;
#9232 = CARTESIAN_POINT ( 'NONE',  ( 31.51612863268893960, -4.239777773060436239, -3.283357778048664688 ) ) ;
#9233 = CARTESIAN_POINT ( 'NONE',  ( -27.17934203385504333, -30.00000000000000355, -0.000000000000000000 ) ) ;
#9234 = EDGE_CURVE ( 'NONE', #15769, #4820, #8504, .T. ) ;
#9235 = CARTESIAN_POINT ( 'NONE',  ( 27.00222791626931595, -2.275731535614434531, -5.783357778048658027 ) ) ;
#9236 = CARTESIAN_POINT ( 'NONE',  ( 29.86122125502053848, -4.439161430227785310, -8.283357778048662468 ) ) ;
#9237 = EDGE_CURVE ( 'NONE', #7716, #16729, #4332, .T. ) ;
#9238 = FILL_AREA_STYLE_COLOUR ( '', #11583 ) ;
#9239 = AXIS2_PLACEMENT_3D ( 'NONE', #222, #4476, #5732 ) ;
#9240 = CARTESIAN_POINT ( 'NONE',  ( 32.04575515724926760, -1.668086104879473730, -5.783357778048658027 ) ) ;
#9241 = CARTESIAN_POINT ( 'NONE',  ( 31.45915434921569798, -2.992700983430681028, -7.939653947423660263 ) ) ;
#9242 = ORIENTED_EDGE ( 'NONE', *, *, #16651, .F. ) ;
#9243 = CARTESIAN_POINT ( 'NONE',  ( 5.500000000000000888, -20.49999999999999645, 13.00000000000000178 ) ) ;
#9244 = CARTESIAN_POINT ( 'NONE',  ( 0.000000000000000000, 0.000000000000000000, 1.102182119232618281E-16 ) ) ;
#9245 = AXIS2_PLACEMENT_3D ( 'NONE', #258, #8783, #11569 ) ;
#9246 = AXIS2_PLACEMENT_3D ( 'NONE', #13277, #13106, #17112 ) ;
#9247 = PRODUCT_DEFINITION_SHAPE ( 'NONE', 'NONE',  #10978 ) ;
#9248 = ORIENTED_EDGE ( 'NONE', *, *, #16533, .F. ) ;
#9249 = CARTESIAN_POINT ( 'NONE',  ( 26.01595305975170547, -2.384361315936983416, 5.783357778048657138 ) ) ;
#9250 = CARTESIAN_POINT ( 'NONE',  ( 30.88125018618674034, -3.062327022369072171, -3.627061608673662896 ) ) ;
#9251 = CARTESIAN_POINT ( 'NONE',  ( 2.500000000000000000, 0.000000000000000000, -3.000000000000000000 ) ) ;
#9252 = CARTESIAN_POINT ( 'NONE',  ( 28.28511899221430070, -4.629050627332469858, -3.283357778048664688 ) ) ;
#9253 = CARTESIAN_POINT ( 'NONE',  ( 25.76524775868382733, -2.816745038626285780, 6.289456735611078209 ) ) ;
#9254 = CARTESIAN_POINT ( 'NONE',  ( 1.257202807339943496, -3.892955774273574310, -3.133250573521610516 ) ) ;
#9255 = CARTESIAN_POINT ( 'NONE',  ( 32.26287188679368967, -2.695996373064596607, -8.283357778048658915 ) ) ;
#9256 = VECTOR ( 'NONE', #12666, 1000.000000000000000 ) ;
#9257 = EDGE_CURVE ( 'NONE', #17832, #13537, #4906, .T. ) ;
#9258 = EDGE_LOOP ( 'NONE', ( #9685, #4208, #3557, #6754 ) ) ;
#9259 = CARTESIAN_POINT ( 'NONE',  ( 0.000000000000000000, 0.000000000000000000, 1.599999999999998979 ) ) ;
#9260 = DIRECTION ( 'NONE',  ( 1.000000000000000000, 0.000000000000000000, 0.000000000000000000 ) ) ;
#9261 = CARTESIAN_POINT ( 'NONE',  ( 0.6448876103708347518, 4.246476118072353145, -0.2256878752776725616 ) ) ;
#9262 = CARTESIAN_POINT ( 'NONE',  ( 46.86575133767496482, -2.390451368237048513, -5.783357778048662468 ) ) ;
#9263 = CARTESIAN_POINT ( 'NONE',  ( 29.04309111455793513, -1.630102785574754742, -5.783357778048658027 ) ) ;
#9264 = AXIS2_PLACEMENT_3D ( 'NONE', #6408, #17226, #16123 ) ;
#9265 = CARTESIAN_POINT ( 'NONE',  ( 32.12473870642251939, -5.420393343910986594, -7.939653947423662927 ) ) ;
#9266 = EDGE_CURVE ( 'NONE', #8870, #9288, #15487, .T. ) ;
#9267 = AXIS2_PLACEMENT_3D ( 'NONE', #17110, #4662, #10190 ) ;
#9268 = LINE ( 'NONE', #6552, #14727 ) ;
#9269 = ORIENTED_EDGE ( 'NONE', *, *, #13314, .F. ) ;
#9270 = CARTESIAN_POINT ( 'NONE',  ( -29.08686357714922011, -14.78463821260646860, -13.41883458853107669 ) ) ;
#9271 = VERTEX_POINT ( 'NONE', #14597 ) ;
#9272 = DIRECTION ( 'NONE',  ( 1.000000000000000000, 0.000000000000000000, 0.000000000000000000 ) ) ;
#9273 = LINE ( 'NONE', #7335, #14831 ) ;
#9274 = CARTESIAN_POINT ( 'NONE',  ( 33.35047706458318828, -2.764833946905070672, -7.939653947423660263 ) ) ;
#9275 =( GEOMETRIC_REPRESENTATION_CONTEXT ( 3 ) GLOBAL_UNCERTAINTY_ASSIGNED_CONTEXT ( ( #9172 ) ) GLOBAL_UNIT_ASSIGNED_CONTEXT ( ( #6254, #2195, #15970 ) ) REPRESENTATION_CONTEXT ( 'NONE', 'WORKASPACE' ) );
#9276 = DIRECTION ( 'NONE',  ( -1.000000000000000000, -0.000000000000000000, -0.000000000000000000 ) ) ;
#9277 = ADVANCED_FACE ( 'NONE', ( #13484 ), #6504, .T. ) ;
#9278 = CARTESIAN_POINT ( 'NONE',  ( 26.47260139170898441, -4.847423203795396596, -3.283357778048664688 ) ) ;
#9279 = CARTESIAN_POINT ( 'NONE',  ( -2.016448651773435938E-27, -20.49999999999999645, 13.00000000000000355 ) ) ;
#9280 = AXIS2_PLACEMENT_3D ( 'NONE', #16366, #2748, #17748 ) ;
#9281 = CARTESIAN_POINT ( 'NONE',  ( 4.000000000000000000, -2.309401076758510918, -3.133295621305383083 ) ) ;
#9282 = CYLINDRICAL_SURFACE ( 'NONE', #15554, 2.000000000000001776 ) ;
#9283 = AXIS2_PLACEMENT_3D ( 'NONE', #1736, #17164, #7537 ) ;
#9284 = CARTESIAN_POINT ( 'NONE',  ( 31.02146712245815507, -5.553315781884258229, -7.939653947423664704 ) ) ;
#9285 = CARTESIAN_POINT ( 'NONE',  ( 33.40301380667672504, -2.758504307001591549, -3.627061608673662896 ) ) ;
#9286 = FACE_OUTER_BOUND ( 'NONE', #6737, .T. ) ;
#9287 = CARTESIAN_POINT ( 'NONE',  ( 31.90644508241650357, -6.373472726347483963, 4.533357778048659803 ) ) ;
#9288 = VERTEX_POINT ( 'NONE', #3690 ) ;
#9289 = EDGE_CURVE ( 'NONE', #11111, #4281, #14175, .T. ) ;
#9290 = VECTOR ( 'NONE', #8971, 1000.000000000000227 ) ;
#9291 = ORIENTED_EDGE ( 'NONE', *, *, #17773, .T. ) ;
#9292 = CARTESIAN_POINT ( 'NONE',  ( 28.89355063163679915, -2.047864499088824175, 5.783357778048668685 ) ) ;
#9293 = CARTESIAN_POINT ( 'NONE',  ( -29.08686357714922011, -14.78463821260646860, 13.41883458853107669 ) ) ;
#9294 = CARTESIAN_POINT ( 'NONE',  ( 20.84394630543432569, -22.08803114836474890, 15.35658910651175013 ) ) ;
#9295 = CIRCLE ( 'NONE', #6404, 0.2500000000000002220 ) ;
#9296 = ORIENTED_EDGE ( 'NONE', *, *, #15901, .T. ) ;
#9297 = AXIS2_PLACEMENT_3D ( 'NONE', #16247, #17722, #16342 ) ;
#9298 = CARTESIAN_POINT ( 'NONE',  ( -38.15522249139979749, -7.597641695372263193, -5.783357778048663356 ) ) ;
#9299 = CARTESIAN_POINT ( 'NONE',  ( 1.500000000000000222, 9.718191103688258892, -2.333127728361106712 ) ) ;
#9300 = LINE ( 'NONE', #10726, #3538 ) ;
#9301 = CARTESIAN_POINT ( 'NONE',  ( 30.81132015408399027, -5.578634341498224458, -3.627061608673668225 ) ) ;
#9302 = CIRCLE ( 'NONE', #5524, 2.000000000000001776 ) ;
#9303 = EDGE_CURVE ( 'NONE', #15953, #15303, #15043, .T. ) ;
#9304 = FACE_OUTER_BOUND ( 'NONE', #10031, .T. ) ;
#9305 = DIRECTION ( 'NONE',  ( 0.9928203230275512992, 0.1196152422706614898, -0.000000000000000000 ) ) ;
#9306 = CARTESIAN_POINT ( 'NONE',  ( -45.50000000000000000, -16.03270077640482683, 8.287981825772241962 ) ) ;
#9307 = LINE ( 'NONE', #14846, #12808 ) ;
#9308 = DIRECTION ( 'NONE',  ( -1.000000000000000000, 0.000000000000000000, 0.000000000000000000 ) ) ;
#9309 = VECTOR ( 'NONE', #1105, 1000.000000000000227 ) ;
#9310 = CARTESIAN_POINT ( 'NONE',  ( 27.41826274939272423, -4.733489685532582314, 3.283357778048664244 ) ) ;
#9311 = VERTEX_POINT ( 'NONE', #14844 ) ;
#9312 = AXIS2_PLACEMENT_3D ( 'NONE', #851, #7835, #2319 ) ;
#9313 = ORIENTED_EDGE ( 'NONE', *, *, #7444, .T. ) ;
#9314 = ADVANCED_FACE ( 'NONE', ( #9044 ), #706, .F. ) ;
#9315 = CARTESIAN_POINT ( 'NONE',  ( 32.01513846370018967, -2.298745344637636912, 6.861505862736165362 ) ) ;
#9316 = CARTESIAN_POINT ( 'NONE',  ( 31.24031073583692475, -4.273008382657478954, 7.939653947423662039 ) ) ;
#9317 = ORIENTED_EDGE ( 'NONE', *, *, #2827, .T. ) ;
#9318 = FACE_OUTER_BOUND ( 'NONE', #15024, .T. ) ;
#9319 = CARTESIAN_POINT ( 'NONE',  ( 33.15485366002904755, -6.560422763297783177, 5.783357778048664244 ) ) ;
#9320 = CARTESIAN_POINT ( 'NONE',  ( 29.26075783691881682, -2.330785036554694489, -4.533357778048659803 ) ) ;
#9322 = CIRCLE ( 'NONE', #1515, 14.00000000000000178 ) ;
#9321 = CARTESIAN_POINT ( 'NONE',  ( 28.41655006632555569, -6.494127376913395366, -4.705209693361169343 ) ) ;
#9323 = DIRECTION ( 'NONE',  ( 0.05980762113533041185, -0.4964101615137758161, 0.8660254037844385966 ) ) ;
#9324 = VERTEX_POINT ( 'NONE', #10389 ) ;
#9325 = ORIENTED_EDGE ( 'NONE', *, *, #6806, .T. ) ;
#9326 = CARTESIAN_POINT ( 'NONE',  ( 31.78252145740879797, -2.026962321187214311, -4.533357778048659803 ) ) ;
#9327 = LINE ( 'NONE', #6603, #6635 ) ;
#9328 = CARTESIAN_POINT ( 'NONE',  ( 17.15697743806116549, -13.99005979112454767, 15.97644891051836957 ) ) ;
#9329 = CARTESIAN_POINT ( 'NONE',  ( 30.19827253897071273, -3.144612341114420673, -7.939653947423660263 ) ) ;
#9330 = CARTESIAN_POINT ( 'NONE',  ( 33.56062403295735663, -2.739515387291123982, -3.627061608673662008 ) ) ;
#9331 = ORIENTED_EDGE ( 'NONE', *, *, #12904, .F. ) ;
#9332 = FACE_OUTER_BOUND ( 'NONE', #3099, .T. ) ;
#9333 = DIRECTION ( 'NONE',  ( -0.1196152422706609625, 0.9928203230275510771, 0.000000000000000000 ) ) ;
#9334 = AXIS2_PLACEMENT_3D ( 'NONE', #12820, #11441, #17007 ) ;
#9335 = EDGE_LOOP ( 'NONE', ( #9977, #8944, #14682, #1300 ) ) ;
#9336 = ADVANCED_FACE ( 'NONE', ( #7687 ), #8953, .F. ) ;
#9337 = CARTESIAN_POINT ( 'NONE',  ( 32.54050588463559990, -2.235448945602741766, 4.705209693361167567 ) ) ;
#9338 = CARTESIAN_POINT ( 'NONE',  ( 29.49337484321020497, -2.602568060005117090, -4.705209693361161349 ) ) ;
#9339 = CARTESIAN_POINT ( 'NONE',  ( -45.00000000000000711, -16.03270077640482683, 5.537981825772250843 ) ) ;
#9340 = CARTESIAN_POINT ( 'NONE',  ( 32.61569110240115776, -6.288022587442930522, 4.533357778048659803 ) ) ;
#9341 = CARTESIAN_POINT ( 'NONE',  ( 26.01652455409633902, -4.902371455920928156, -5.783357778048663356 ) ) ;
#9342 = CARTESIAN_POINT ( 'NONE',  ( 1.360615521534834782, -4.061278559077730499, -3.205052026701941781 ) ) ;
#9343 = UNCERTAINTY_MEASURE_WITH_UNIT (LENGTH_MEASURE( 1.000000000000000082E-05 ), #3239, 'distance_accuracy_value', 'NONE');
#9344 = EDGE_CURVE ( 'NONE', #14154, #16640, #17521, .T. ) ;
#9345 = CARTESIAN_POINT ( 'NONE',  ( 33.01342578063301403, -4.059383036018435753, -8.283357778048662468 ) ) ;
#9346 = PRODUCT_RELATED_PRODUCT_CATEGORY ( 'part', '', ( #13747 ) ) ;
#9347 = EDGE_LOOP ( 'NONE', ( #15123, #12404, #5735, #14876 ) ) ;
#9348 = DIRECTION ( 'NONE',  ( 1.000000000000000000, 0.000000000000000000, 0.000000000000000000 ) ) ;
#9349 = CARTESIAN_POINT ( 'NONE',  ( 26.27285561281999193, -7.029948842322393254, -4.710679390969556124 ) ) ;
#9350 = DIRECTION ( 'NONE',  ( 0.000000000000000000, 0.000000000000000000, -1.000000000000000000 ) ) ;
#9351 = DIRECTION ( 'NONE',  ( -0.000000000000000000, -0.000000000000000000, 1.000000000000000000 ) ) ;
#9352 = CARTESIAN_POINT ( 'NONE',  ( 26.89670596474818609, -7.703954147932045693, -5.783357778048669573 ) ) ;
#9353 = CARTESIAN_POINT ( 'NONE',  ( 32.65880277236253448, -4.102108105263264193, -7.939653947423662039 ) ) ;
#9354 = EDGE_CURVE ( 'NONE', #14350, #14070, #4859, .T. ) ;
#9355 = CIRCLE ( 'NONE', #2425, 2.749999999999995559 ) ;
#9356 = ORIENTED_EDGE ( 'NONE', *, *, #2968, .T. ) ;
#9357 = CARTESIAN_POINT ( 'NONE',  ( 45.50000000000000000, -16.03270077640482683, -5.537981825772250843 ) ) ;
#9358 = CARTESIAN_POINT ( 'NONE',  ( 3.679171394226031122, 2.494631558665831861, -0.3503314178412501589 ) ) ;
#9359 = VERTEX_POINT ( 'NONE', #5123 ) ;
#9360 = CARTESIAN_POINT ( 'NONE',  ( 11.38175538881591287, -22.33742387525453665, 16.67884400577319681 ) ) ;
#9361 = LINE ( 'NONE', #1037, #15111 ) ;
#9362 = DIRECTION ( 'NONE',  ( -0.1196152422706614760, 0.9928203230275510771, 0.000000000000000000 ) ) ;
#9363 = CARTESIAN_POINT ( 'NONE',  ( 33.17547354829333273, -5.293800545841212291, -3.627061608673667781 ) ) ;
#9364 = CARTESIAN_POINT ( 'NONE',  ( 31.87265695910486230, -5.650636735497883478, 3.283357778048663356 ) ) ;
#9365 = DIRECTION ( 'NONE',  ( -0.1196152422706610735, 0.9928203230275511881, 0.000000000000000000 ) ) ;
#9366 = CARTESIAN_POINT ( 'NONE',  ( 33.59503905791412137, -1.808589744724287129, -4.533357778048659803 ) ) ;
#9367 = CARTESIAN_POINT ( 'NONE',  ( 26.01595305975170547, -2.384361315936983416, -5.783357778048670461 ) ) ;
#9368 = CARTESIAN_POINT ( 'NONE',  ( 31.63243098167119172, -2.771952051906466874, 3.283357778048666464 ) ) ;
#9369 = ORIENTED_EDGE ( 'NONE', *, *, #6043, .T. ) ;
#9370 = EDGE_LOOP ( 'NONE', ( #6819, #2799, #10895, #12668, #7491 ) ) ;
#9371 = ADVANCED_FACE ( 'NONE', ( #17319 ), #14494, .F. ) ;
#9372 = CARTESIAN_POINT ( 'NONE',  ( 29.54591158530375239, -2.596238420101622868, 4.705209693361168455 ) ) ;
#9373 = CARTESIAN_POINT ( 'NONE',  ( -19.22778933661430756, -11.21824206523807099, 15.64718775662042560 ) ) ;
#9374 = CARTESIAN_POINT ( 'NONE',  ( 25.20704250852812933, -22.06899625087205763, 14.42769424659100785 ) ) ;
#9375 = EDGE_LOOP ( 'NONE', ( #13688, #9607, #4317, #3867 ) ) ;
#9376 = CYLINDRICAL_SURFACE ( 'NONE', #16893, 2.000000000000001776 ) ;
#9377 = CYLINDRICAL_SURFACE ( 'NONE', #13622, 2.500000000000001776 ) ;
#9378 = VERTEX_POINT ( 'NONE', #16044 ) ;
#9379 = CARTESIAN_POINT ( 'NONE',  ( 32.96459815279162342, -1.884545423566157174, -4.533357778048659803 ) ) ;
#9380 = EDGE_CURVE ( 'NONE', #15303, #13014, #791, .T. ) ;
#9381 = CARTESIAN_POINT ( 'NONE',  ( 29.52399153675929355, -1.971908820246954130, -5.783357778048658027 ) ) ;
#9382 = AXIS2_PLACEMENT_3D ( 'NONE', #1324, #9722, #12296 ) ;
#9383 = DIRECTION ( 'NONE',  ( -0.9928203230275514102, -0.1196152422706598939, -0.000000000000000000 ) ) ;
#9384 = CARTESIAN_POINT ( 'NONE',  ( 29.70732014299206369, -2.276983097582480742, 4.533357778048667797 ) ) ;
#9385 =( NAMED_UNIT ( * ) PLANE_ANGLE_UNIT ( ) SI_UNIT ( $, .RADIAN. ) );
#9386 = CARTESIAN_POINT ( 'NONE',  ( 26.99805802979993885, -6.665027654307603022, 6.861505862736158257 ) ) ;
#9387 = PRODUCT_DEFINITION_SHAPE ( 'NONE', 'NONE',  #5901 ) ;
#9388 = ORIENTED_EDGE ( 'NONE', *, *, #2701, .F. ) ;
#9389 = FACE_OUTER_BOUND ( 'NONE', #13737, .T. ) ;
#9390 = DIRECTION ( 'NONE',  ( 0.000000000000000000, 0.000000000000000000, 1.000000000000000000 ) ) ;
#9391 = CARTESIAN_POINT ( 'NONE',  ( 32.82963640218302004, -5.962437625020304388, 6.861505862736157368 ) ) ;
#9392 = CARTESIAN_POINT ( 'NONE',  ( 29.42969845347704450, -5.944964990802679594, 3.283357778048663800 ) ) ;
#9393 = ORIENTED_EDGE ( 'NONE', *, *, #11616, .F. ) ;
#9394 = ORIENTED_EDGE ( 'NONE', *, *, #7691, .T. ) ;
#9395 = EDGE_CURVE ( 'NONE', #10652, #17258, #1027, .T. ) ;
#9396 = ORIENTED_EDGE ( 'NONE', *, *, #6529, .T. ) ;
#9397 = CARTESIAN_POINT ( 'NONE',  ( 33.19286683830256379, -2.783822866615540903, 3.627061608673666893 ) ) ;
#9398 = CYLINDRICAL_SURFACE ( 'NONE', #4696, 2.500000000000001776 ) ;
#9399 = CARTESIAN_POINT ( 'NONE',  ( 30.30787278169304244, -6.266260340387784566, 6.861505862736157368 ) ) ;
#9400 = VERTEX_POINT ( 'NONE', #5042 ) ;
#9401 = CARTESIAN_POINT ( 'NONE',  ( 10.47816170930907553, -0.6768509389586216951, -7.794427190999915211 ) ) ;
#9402 = DIRECTION ( 'NONE',  ( 0.9928203230275510771, 0.1196152422706609902, 4.006172263299092517E-17 ) ) ;
#9403 = CARTESIAN_POINT ( 'NONE',  ( 34.91377932259078420, -11.86950488720510322, 11.57182824616228878 ) ) ;
#9404 = CARTESIAN_POINT ( 'NONE',  ( 28.91547068018125799, -2.672194098943493135, -6.861505862736158257 ) ) ;
#9405 = CARTESIAN_POINT ( 'NONE',  ( 29.74794773085836397, -1.934729659147405689, 6.453230759126469707 ) ) ;
#9406 = ADVANCED_FACE ( 'NONE', ( #10565, #16129 ), #2430, .T. ) ;
#9407 = CARTESIAN_POINT ( 'NONE',  ( 32.77701044293393551, -4.087866415376695706, -3.283357778048664688 ) ) ;
#9408 = CARTESIAN_POINT ( 'NONE',  ( 0.000000000000000000, 0.000000000000000000, -8.700000000000001066 ) ) ;
#9409 = CARTESIAN_POINT ( 'NONE',  ( 18.32916366311290091, -12.06017896066153128, -15.79554754021495633 ) ) ;
#9410 = CARTESIAN_POINT ( 'NONE',  ( 27.95350797341489368, -12.38528642892598342, 13.73189064827997541 ) ) ;
#9411 = SURFACE_STYLE_FILL_AREA ( #16335 ) ;
#9412 = EDGE_CURVE ( 'NONE', #1473, #8190, #11666, .T. ) ;
#9413 = CARTESIAN_POINT ( 'NONE',  ( 30.18087924896149588, -5.654590020340094725, -3.627061608673668225 ) ) ;
#9414 = CARTESIAN_POINT ( 'NONE',  ( 29.78250536075762867, -6.329556739422670830, -6.861505862736167138 ) ) ;
#9415 = EDGE_LOOP ( 'NONE', ( #10775, #281 ) ) ;
#9416 = CARTESIAN_POINT ( 'NONE',  ( -27.17934203385504333, -30.00000000000000355, 13.93658524716016878 ) ) ;
#9417 = DIRECTION ( 'NONE',  ( -0.9928203230275512992, -0.1196152422706610180, -4.006172263299093133E-17 ) ) ;
#9418 = ORIENTED_EDGE ( 'NONE', *, *, #8369, .T. ) ;
#9419 = CARTESIAN_POINT ( 'NONE',  ( 30.76748005699505129, -4.329975141788874993, 3.627061608673664228 ) ) ;
#9420 = CARTESIAN_POINT ( 'NONE',  ( 26.84461768998868436, -2.294720455324902542, -5.783357778048658915 ) ) ;
#9421 = CARTESIAN_POINT ( 'NONE',  ( 1.746467850512308208E-21, -1.591841644184202181E-21, -6.005572809000082835 ) ) ;
#9422 = CARTESIAN_POINT ( 'NONE',  ( 28.19013153391124860, -7.158573733970061248, 5.783357778048669573 ) ) ;
#9423 = CARTESIAN_POINT ( 'NONE',  ( 0.000000000000000000, 0.000000000000000000, -4.000000000000000000 ) ) ;
#9424 = DIRECTION ( 'NONE',  ( -0.1196152422706611984, 0.9928203230275510771, 0.000000000000000000 ) ) ;
#9425 = CARTESIAN_POINT ( 'NONE',  ( 0.000000000000000000, 0.000000000000000000, 4.000000000000000000 ) ) ;
#9426 = CARTESIAN_POINT ( 'NONE',  ( 29.67353201968042598, -1.554147106732884920, -5.783357778048658027 ) ) ;
#9427 = ORIENTED_EDGE ( 'NONE', *, *, #13074, .T. ) ;
#9428 = ADVANCED_FACE ( 'NONE', ( #3422 ), #10297, .T. ) ;
#9429 = VERTEX_POINT ( 'NONE', #8214 ) ;
#9430 = CARTESIAN_POINT ( 'NONE',  ( 33.40754056521197413, -5.892811586081919906, -6.861505862736166250 ) ) ;
#9431 = CARTESIAN_POINT ( 'NONE',  ( 31.68992120585416217, -1.700760206360153015, 5.783357778048662468 ) ) ;
#9432 = CARTESIAN_POINT ( 'NONE',  ( 31.71807556108801407, -1.697368162559112825, -5.113484796970855228 ) ) ;
#9433 = CARTESIAN_POINT ( 'NONE',  ( -0.1756478951291671753, 4.720212513052427283, -3.169390900447852655 ) ) ;
#9434 = CARTESIAN_POINT ( 'NONE',  ( -3.453019673806803524, -2.625200315327865130, -3.235259548910208505 ) ) ;
#9435 = CARTESIAN_POINT ( 'NONE',  ( 32.77709966008947617, -5.968767264923789284, -6.861505862736166250 ) ) ;
#9436 = ADVANCED_FACE ( 'NONE', ( #5384 ), #5398, .T. ) ;
#9437 = ORIENTED_EDGE ( 'NONE', *, *, #7691, .F. ) ;
#9438 = CARTESIAN_POINT ( 'NONE',  ( -13.65694651542706595, -25.37101204406941335, 16.45580752066269881 ) ) ;
#9439 =( BOUNDED_CURVE ( )  B_SPLINE_CURVE ( 2, ( #6224, #14487, #7683, #13208, #2249, #7763, #3507, #784, #7859 ),
 .UNSPECIFIED., .F., .T. ) 
 B_SPLINE_CURVE_WITH_KNOTS ( ( 3, 2, 2, 2, 3 ),
 ( 0.4038461538461538547, 0.4102564102564102422, 0.4230769230769230727, 0.4358974358974359031, 0.4423076923076923461 ),
 .UNSPECIFIED. ) 
 CURVE ( )  GEOMETRIC_REPRESENTATION_ITEM ( )  RATIONAL_B_SPLINE_CURVE ( ( 0.9330127018922194093, 0.9330127018922196314, 1.000000000000000000, 0.8660254037844387076, 1.000000000000000000, 0.8660254037844387076, 1.000000000000000000, 0.9330127018922190762, 0.9330127018922194093 ) ) 
 REPRESENTATION_ITEM ( '' )  );
#9440 = ORIENTED_EDGE ( 'NONE', *, *, #12115, .T. ) ;
#9441 = DIRECTION ( 'NONE',  ( -0.1196152422706611984, 0.9928203230275510771, 0.000000000000000000 ) ) ;
#9442 = ORIENTED_EDGE ( 'NONE', *, *, #12736, .T. ) ;
#9443 = DIRECTION ( 'NONE',  ( 0.000000000000000000, 0.000000000000000000, 1.000000000000000000 ) ) ;
#9444 = CARTESIAN_POINT ( 'NONE',  ( 30.43486631442457835, -6.877930660435475296, -5.783357778048669573 ) ) ;
#9445 = ORIENTED_EDGE ( 'NONE', *, *, #9478, .F. ) ;
#9446 = CARTESIAN_POINT ( 'NONE',  ( -1.917618200156724081E-28, -7.000000000000001776, -6.000000000000000000 ) ) ;
#9447 = EDGE_CURVE ( 'NONE', #15376, #16997, #2862, .T. ) ;
#9448 = CARTESIAN_POINT ( 'NONE',  ( 33.40301380667672504, -2.758504307001591549, -3.627061608673662896 ) ) ;
#9449 = EDGE_CURVE ( 'NONE', #13433, #2702, #3872, .T. ) ;
#9450 = DIRECTION ( 'NONE',  ( 0.000000000000000000, 0.000000000000000000, -1.000000000000000000 ) ) ;
#9451 = CARTESIAN_POINT ( 'NONE',  ( 13.65694651542703397, -25.37101204406936361, -16.45580752066269881 ) ) ;
#9452 = CARTESIAN_POINT ( 'NONE',  ( 33.45617745041539592, -1.098413033681664430, -5.783357778048658027 ) ) ;
#9453 = DIRECTION ( 'NONE',  ( 1.000000000000000000, 0.000000000000000000, 0.000000000000000000 ) ) ;
#9454 = CARTESIAN_POINT ( 'NONE',  ( 33.01342578063301403, -4.059383036018435753, 3.283357778048664244 ) ) ;
#9455 = ORIENTED_EDGE ( 'NONE', *, *, #4408, .T. ) ;
#9456 = CARTESIAN_POINT ( 'NONE',  ( 26.13613979636700080, -5.895191778948487560, -5.783357778048664244 ) ) ;
#9457 = CIRCLE ( 'NONE', #10888, 12.50000000000000000 ) ;
#9458 = CARTESIAN_POINT ( 'NONE',  ( 31.04338717100262102, -6.177645381738930297, 4.705209693361159573 ) ) ;
#9459 = CARTESIAN_POINT ( 'NONE',  ( -14.00000000000000178, 0.000000000000000000, -8.700000000000001066 ) ) ;
#9460 = CARTESIAN_POINT ( 'NONE',  ( 2.500000000000000000, 1.768423874527822903, -1.021000000000002350 ) ) ;
#9461 = ORIENTED_EDGE ( 'NONE', *, *, #9257, .T. ) ;
#9462 = LINE ( 'NONE', #7761, #5274 ) ;
#9463 = DIRECTION ( 'NONE',  ( 0.1196152422706590474, -0.9928203230275514102, 0.000000000000000000 ) ) ;
#9464 = FACE_OUTER_BOUND ( 'NONE', #12194, .T. ) ;
#9465 = CARTESIAN_POINT ( 'NONE',  ( 28.51709679197739078, -3.347160818026084339, -3.627061608673662008 ) ) ;
#9466 = PLANE ( 'NONE',  #547 ) ;
#9467 = CARTESIAN_POINT ( 'NONE',  ( 29.98133424373737199, -5.878503772023492502, 3.283357778048663356 ) ) ;
#9468 = CARTESIAN_POINT ( 'NONE',  ( 0.000000000000000000, 0.000000000000000000, 0.000000000000000000 ) ) ;
#9469 = CARTESIAN_POINT ( 'NONE',  ( 26.66961417369883591, -4.823687054261037055, 7.939653947423662039 ) ) ;
#9470 = CARTESIAN_POINT ( 'NONE',  ( 30.25080928106424594, -3.138282701210941994, 7.939653947423664704 ) ) ;
#9471 = EDGE_CURVE ( 'NONE', #8870, #10739, #13837, .T. ) ;
#9472 = PLANE ( 'NONE',  #11938 ) ;
#9473 = CARTESIAN_POINT ( 'NONE',  ( 26.01652455409633902, -4.902371455920926380, -5.783357778048663356 ) ) ;
#9474 = CARTESIAN_POINT ( 'NONE',  ( 32.67619606237177265, -1.592130426037603907, 5.783357778048668685 ) ) ;
#9475 = B_SPLINE_CURVE_WITH_KNOTS ( 'NONE', 3,
 ( #3674, #11912, #8103, #17760, #14908, #3939, #7849, #13638, #12279, #16024, #2490, #17587, #17501, #5107, #16200, #3765, #9539, #4118, #6832, #2671, #14083, #12358, #10887, #16632, #15352, #1489, #6918, #8366, #2760, #11149, #15087, #13809, #12714, #8200, #5546, #13896, #9626, #2931, #7116, #37, #8551, #9801, #4290 ),
 .UNSPECIFIED., .F., .F.,
 ( 4, 2, 2, 1, 2, 2, 2, 2, 2, 2, 2, 2, 2, 2, 2, 2, 2, 2, 2, 2, 2, 4 ),
 ( 0.01976987703536532692, 0.02100501831352976842, 0.02162258895261198396, 0.02224015959169420298, 0.02285773023077641852, 0.02347530086985863407, 0.02471044214802306516, 0.02594558342618749971, 0.02718072470435193080, 0.02779829534343414288, 0.02841586598251635495, 0.02965100726068079298, 0.03088614853884522754, 0.03150371917792745002, 0.03212128981700967945, 0.03335643109517413829, 0.03459157237333859714, 0.03582671365150305598, 0.03644428429058528540, 0.03706185492966751482, 0.03829699620783197367, 0.03953213748599642557 ),
 .UNSPECIFIED. ) ;
#9476 = CARTESIAN_POINT ( 'NONE',  ( 28.04870365451522218, -4.657534006690712935, 3.283357778048664244 ) ) ;
#9477 = VERTEX_POINT ( 'NONE', #53 ) ;
#9478 = EDGE_CURVE ( 'NONE', #2213, #15493, #4624, .T. ) ;
#9479 = VERTEX_POINT ( 'NONE', #13913 ) ;
#9480 = VERTEX_POINT ( 'NONE', #15007 ) ;
#9481 = CARTESIAN_POINT ( 'NONE',  ( 32.16857880351144416, -6.669052543620333395, 5.783357778048658027 ) ) ;
#9482 = PLANE ( 'NONE',  #13676 ) ;
#9483 = VERTEX_POINT ( 'NONE', #8121 ) ;
#9484 = CARTESIAN_POINT ( 'NONE',  ( 28.93739072872572393, -3.296523698798161650, 3.627061608673666449 ) ) ;
#9485 = CARTESIAN_POINT ( 'NONE',  ( 31.27600417729400917, -6.449428405189353342, -7.033357778048666908 ) ) ;
#9486 = AXIS2_PLACEMENT_3D ( 'NONE', #6243, #13413, #11856 ) ;
#9487 = CYLINDRICAL_SURFACE ( 'NONE', #2033, 6.249999999999998224 ) ;
#9488 = PLANE ( 'NONE',  #8750 ) ;
#9489 = CIRCLE ( 'NONE', #3434, 13.00000000000000178 ) ;
#9490 = CARTESIAN_POINT ( 'NONE',  ( -2.016448651773435938E-27, -20.49999999999999645, -13.00000000000000178 ) ) ;
#9491 = CARTESIAN_POINT ( 'NONE',  ( 28.13873763417254992, -3.192873105281056390, -3.283357778048662023 ) ) ;
#9492 = CARTESIAN_POINT ( 'NONE',  ( -3.248936832696171617, -20.49508120620799900, -78.00000000000000000 ) ) ;
#9493 = CARTESIAN_POINT ( 'NONE',  ( 19.91392456697921531, -10.76755109436559010, -15.52754005891982736 ) ) ;
#9494 = CARTESIAN_POINT ( 'NONE',  ( 26.90109536843240789, -7.313877135454839973, 6.453230759126468818 ) ) ;
#9495 = ORIENTED_EDGE ( 'NONE', *, *, #16582, .F. ) ;
#9496 = EDGE_CURVE ( 'NONE', #1259, #9479, #16499, .T. ) ;
#9497 = CARTESIAN_POINT ( 'NONE',  ( 31.04338717100262102, -6.177645381738930297, -6.861505862736167138 ) ) ;
#9498 = CARTESIAN_POINT ( 'NONE',  ( 29.67743187657054449, -6.342216019229654833, -4.705209693361169343 ) ) ;
#9499 = DIRECTION ( 'NONE',  ( 0.6000000000000001998, -0.7999999999999999334, 0.000000000000000000 ) ) ;
#9500 = DIRECTION ( 'NONE',  ( -0.1196152422706611984, 0.9928203230275511881, 0.000000000000000000 ) ) ;
#9501 = CIRCLE ( 'NONE', #3135, 2.500000000000000444 ) ;
#9502 = ADVANCED_FACE ( 'NONE', ( #17779 ), #6581, .T. ) ;
#9503 = ORIENTED_EDGE ( 'NONE', *, *, #14916, .T. ) ;
#9504 = CARTESIAN_POINT ( 'NONE',  ( 32.14665875496697822, -6.044722943765660439, 4.705209693361160461 ) ) ;
#9505 = CARTESIAN_POINT ( 'NONE',  ( 26.88845778707760914, -3.543379655034240905, -7.939653947423660263 ) ) ;
#9506 = FACE_OUTER_BOUND ( 'NONE', #944, .T. ) ;
#9507 = FACE_OUTER_BOUND ( 'NONE', #11969, .T. ) ;
#9508 = CARTESIAN_POINT ( 'NONE',  ( 28.25893984004492765, -6.513116296623863377, -4.705209693361168455 ) ) ;
#9509 = CARTESIAN_POINT ( 'NONE',  ( 0.000000000000000000, 0.000000000000000000, 0.000000000000000000 ) ) ;
#9510 = FACE_OUTER_BOUND ( 'NONE', #5368, .T. ) ;
#9511 = CIRCLE ( 'NONE', #5176, 14.00000000000000178 ) ;
#9512 = LINE ( 'NONE', #17821, #16286 ) ;
#9513 = CARTESIAN_POINT ( 'NONE',  ( 29.98133424373737910, -5.878503772023492502, -8.283357778048662468 ) ) ;
#9514 = ORIENTED_EDGE ( 'NONE', *, *, #4609, .T. ) ;
#9515 = CARTESIAN_POINT ( 'NONE',  ( 31.88814493096863956, -1.687075024589942851, -5.783357778048658027 ) ) ;
#9516 = FACE_OUTER_BOUND ( 'NONE', #6514, .T. ) ;
#9517 = CARTESIAN_POINT ( 'NONE',  ( 30.08145424927873535, -6.930706697444451336, -5.783357778048663356 ) ) ;
#9518 = FACE_OUTER_BOUND ( 'NONE', #11290, .T. ) ;
#9519 = CARTESIAN_POINT ( 'NONE',  ( -4.235887314095728939, -2.417314327725974543, -3.451162025751987272 ) ) ;
#9520 = CARTESIAN_POINT ( 'NONE',  ( 29.39282811755836988, -5.749534618892433002, -3.627061608673667781 ) ) ;
#9521 = AXIS2_PLACEMENT_3D ( 'NONE', #17338, #4968, #3628 ) ;
#9522 = VERTEX_POINT ( 'NONE', #5211 ) ;
#9523 = DIRECTION ( 'NONE',  ( 0.1414213562373112243, -0.9899494936611663576, 0.000000000000000000 ) ) ;
#9524 = EDGE_CURVE ( 'NONE', #16241, #9967, #9640, .T. ) ;
#9525 = ORIENTED_EDGE ( 'NONE', *, *, #9618, .T. ) ;
#9526 = CARTESIAN_POINT ( 'NONE',  ( 26.01652455409633902, -4.902371455920928156, -5.783357778048663356 ) ) ;
#9527 = EDGE_LOOP ( 'NONE', ( #2063, #9427, #7099, #13832 ) ) ;
#9528 = VECTOR ( 'NONE', #15346, 1000.000000000000000 ) ;
#9529 = PRODUCT_DEFINITION_SHAPE ( 'NONE', 'NONE',  #12337 ) ;
#9530 = CARTESIAN_POINT ( 'NONE',  ( 30.39102621733566423, -5.629271460726127607, -7.939653947423662927 ) ) ;
#9531 = VERTEX_POINT ( 'NONE', #10818 ) ;
#9532 = FACE_BOUND ( 'NONE', #7663, .T. ) ;
#9533 = ORIENTED_EDGE ( 'NONE', *, *, #194, .F. ) ;
#9534 = VECTOR ( 'NONE', #12098, 1000.000000000000000 ) ;
#9535 = CARTESIAN_POINT ( 'NONE',  ( 26.87785582392756467, -3.344784462964796479, -3.283357778048662023 ) ) ;
#9536 = CARTESIAN_POINT ( 'NONE',  ( 4.154306624731438191, -2.398490048084426896, -3.421999068284419465 ) ) ;
#9537 = FACE_OUTER_BOUND ( 'NONE', #6637, .T. ) ;
#9538 = CARTESIAN_POINT ( 'NONE',  ( 27.86926259684567597, -5.933094176093606897, -7.939653947423664704 ) ) ;
#9539 = CARTESIAN_POINT ( 'NONE',  ( 25.20704250852812933, -22.06899625087205763, -14.42769424659100785 ) ) ;
#9540 =( BOUNDED_CURVE ( )  B_SPLINE_CURVE ( 3, ( #14729, #13092, #2313, #17196 ),
 .UNSPECIFIED., .F., .T. ) 
 B_SPLINE_CURVE_WITH_KNOTS ( ( 4, 4 ),
 ( 1.316154292592045083, 1.436990331221392081 ),
 .UNSPECIFIED. ) 
 CURVE ( )  GEOMETRIC_REPRESENTATION_ITEM ( )  RATIONAL_B_SPLINE_CURVE ( ( 1.000000000000000000, 0.9987835910734581546, 0.9987835910734581546, 1.000000000000000000 ) ) 
 REPRESENTATION_ITEM ( '' )  );
#9541 = ADVANCED_FACE ( 'NONE', ( #10730 ), #13887, .T. ) ;
#9542 = CARTESIAN_POINT ( 'NONE',  ( 29.14753769709988518, -3.271205139184214516, 7.939653947423664704 ) ) ;
#9543 = CARTESIAN_POINT ( 'NONE',  ( 9.750000000000010658, 3.897114317029950037, -3.000000000000002665 ) ) ;
#9544 = CARTESIAN_POINT ( 'NONE',  ( 28.75424055680402802, -6.753251120556833520, 4.533357778048659803 ) ) ;
#9545 = ORIENTED_EDGE ( 'NONE', *, *, #3902, .F. ) ;
#9546 = SURFACE_STYLE_USAGE ( .BOTH. , #6498 ) ;
#9547 = ORIENTED_EDGE ( 'NONE', *, *, #15251, .F. ) ;
#9548 = CARTESIAN_POINT ( 'NONE',  ( 25.93714794488954212, -2.393855775999666591, 5.783357778048667797 ) ) ;
#9549 = EDGE_LOOP ( 'NONE', ( #17563, #7586, #1112, #10588 ) ) ;
#9550 = CARTESIAN_POINT ( 'NONE',  ( 0.000000000000000000, 0.000000000000000000, 0.000000000000000000 ) ) ;
#9551 = CIRCLE ( 'NONE', #6388, 6.000000000000000888 ) ;
#9552 = CARTESIAN_POINT ( 'NONE',  ( 30.19827253897071273, -3.144612341114420673, -7.939653947423660263 ) ) ;
#9553 = LINE ( 'NONE', #6845, #6622 ) ;
#9554 = CARTESIAN_POINT ( 'NONE',  ( 27.80031630502317341, -2.169380783275094426, 5.113484796970861446 ) ) ;
#9555 = CARTESIAN_POINT ( 'NONE',  ( 25.77727942049545717, -5.625018267156629115, 3.627061608673662452 ) ) ;
#9556 = CARTESIAN_POINT ( 'NONE',  ( 29.38830135902312080, -2.615227339812091767, 4.705209693361167567 ) ) ;
#9557 = DIRECTION ( 'NONE',  ( -0.000000000000000000, -0.000000000000000000, 1.000000000000000000 ) ) ;
#9558 = CARTESIAN_POINT ( 'NONE',  ( 32.21340264088064487, -1.637691031382005669, 5.113484796970859669 ) ) ;
#9559 = CARTESIAN_POINT ( 'NONE',  ( 32.93018312783485158, -2.815471066132994249, 7.939653947423664704 ) ) ;
#9560 =( BOUNDED_CURVE ( )  B_SPLINE_CURVE ( 2, ( #8538, #15518, #9968, #11420, #5980, #8446, #3100, #196, #9782 ),
 .UNSPECIFIED., .F., .T. ) 
 B_SPLINE_CURVE_WITH_KNOTS ( ( 3, 2, 2, 2, 3 ),
 ( 0.8653846153846154188, 0.8717948717948718063, 0.8846153846153845812, 0.8974358974358974672, 0.9038461538461538547 ),
 .UNSPECIFIED. ) 
 CURVE ( )  GEOMETRIC_REPRESENTATION_ITEM ( )  RATIONAL_B_SPLINE_CURVE ( ( 0.9330127018922192983, 0.9330127018922198534, 1.000000000000000000, 0.8660254037844387076, 1.000000000000000000, 0.8660254037844387076, 1.000000000000000000, 0.9330127018922194093, 0.9330127018922194093 ) ) 
 REPRESENTATION_ITEM ( '' )  );
#9561 = AXIS2_PLACEMENT_3D ( 'NONE', #4197, #15246, #2825 ) ;
#9562 = ORIENTED_EDGE ( 'NONE', *, *, #16936, .T. ) ;
#9563 = VERTEX_POINT ( 'NONE', #12295 ) ;
#9564 = CARTESIAN_POINT ( 'NONE',  ( 30.65370992780335868, -5.597623261208691581, 7.939653947423658487 ) ) ;
#9565 = EDGE_LOOP ( 'NONE', ( #14077, #6307, #14391, #11517, #1632, #11250, #4718, #6108, #4154, #16514, #8630, #15363, #15709, #15638, #5870, #113, #1628, #7036, #14770, #13032, #8452, #16621, #3363, #993, #14757, #12974, #146, #5712 ) ) ;
#9566 = CARTESIAN_POINT ( 'NONE',  ( 30.15443244188179150, -1.895953141405083864, 5.783357778048668685 ) ) ;
#9567 = CARTESIAN_POINT ( 'NONE',  ( 0.000000000000000000, 0.000000000000000000, -2.000000000000000000 ) ) ;
#9568 = FACE_OUTER_BOUND ( 'NONE', #10087, .T. ) ;
#9569 = CARTESIAN_POINT ( 'NONE',  ( 33.24613200752366282, -6.212066908601060256, -7.033357778048666908 ) ) ;
#9570 = CARTESIAN_POINT ( 'NONE',  ( -20.00000000000000355, 7.999999999999996447, 6.000000000000000000 ) ) ;
#9571 = CARTESIAN_POINT ( 'NONE',  ( -50.00000000000000000, -16.03270077640482683, 5.537981825772250843 ) ) ;
#9572 = CARTESIAN_POINT ( 'NONE',  ( 30.41656616297672500, -2.191532958677927745, -7.033357778048658027 ) ) ;
#9573 = FACE_OUTER_BOUND ( 'NONE', #1677, .T. ) ;
#9574 = CARTESIAN_POINT ( 'NONE',  ( 20.00000000000000355, -30.00000000000000355, 17.00000000000000000 ) ) ;
#9575 = CARTESIAN_POINT ( 'NONE',  ( 25.76366024945007638, -10.60870341083598056, 14.29366788170017699 ) ) ;
#9576 = ORIENTED_EDGE ( 'NONE', *, *, #13213, .F. ) ;
#9577 = CARTESIAN_POINT ( 'NONE',  ( 28.28955653359400557, -5.882457056865704637, -3.627061608673668225 ) ) ;
#9578 = CARTESIAN_POINT ( 'NONE',  ( 27.00222791626931240, -2.275731535614434531, -5.783357778048658915 ) ) ;
#9579 = VECTOR ( 'NONE', #16948, 1000.000000000000000 ) ;
#9580 = EDGE_LOOP ( 'NONE', ( #2065, #346, #12822, #11635, #7098 ) ) ;
#9581 = DIRECTION ( 'NONE',  ( -0.000000000000000000, -0.000000000000000000, 1.000000000000000000 ) ) ;
#9582 = CARTESIAN_POINT ( 'NONE',  ( 31.68992120585416217, -1.700760206360153015, -5.783357778048664244 ) ) ;
#9583 = ORIENTED_EDGE ( 'NONE', *, *, #8718, .T. ) ;
#9584 = ORIENTED_EDGE ( 'NONE', *, *, #16567, .T. ) ;
#9585 = CARTESIAN_POINT ( 'NONE',  ( 31.51621784984448738, -6.120678622607529817, 4.705209693361160461 ) ) ;
#9586 = CIRCLE ( 'NONE', #2393, 2.749999999999988454 ) ;
#9587 = CARTESIAN_POINT ( 'NONE',  ( 28.75786045390062995, -2.691183018653962034, -6.861505862736159145 ) ) ;
#9588 = EDGE_CURVE ( 'NONE', #4167, #6841, #7713, .T. ) ;
#9589 = CARTESIAN_POINT ( 'NONE',  ( 25.87953856062030766, -3.765371892057810754, -3.950981403410641857 ) ) ;
#9590 = CARTESIAN_POINT ( 'NONE',  ( -25.74999999999998934, -16.21813761408365195, 13.00000000000000355 ) ) ;
#9591 = CARTESIAN_POINT ( 'NONE',  ( 28.99445422935450267, -6.424501337975009996, -6.861505862736166250 ) ) ;
#9592 = DIRECTION ( 'NONE',  ( -0.1196152422706626278, 0.9928203230275510771, 0.000000000000000000 ) ) ;
#9593 = PLANE ( 'NONE',  #14527 ) ;
#9594 = CARTESIAN_POINT ( 'NONE',  ( 0.000000000000000000, 0.000000000000000000, -4.184454397937119374 ) ) ;
#9595 = CARTESIAN_POINT ( 'NONE',  ( 28.69037342443288452, -3.126411886501869741, -3.283357778048662023 ) ) ;
#9596 = EDGE_CURVE ( 'NONE', #8696, #1034, #1444, .T. ) ;
#9597 = ORIENTED_EDGE ( 'NONE', *, *, #12618, .T. ) ;
#9598 = FACE_OUTER_BOUND ( 'NONE', #815, .T. ) ;
#9599 = VECTOR ( 'NONE', #7661, 1000.000000000000000 ) ;
#9600 = CARTESIAN_POINT ( 'NONE',  ( 30.63309003953906995, -6.864245478665264244, -5.783357778048663356 ) ) ;
#9601 = CARTESIAN_POINT ( 'NONE',  ( 2.500000000000000888, 3.061616997868384127E-16, -4.674599999999997202 ) ) ;
#9602 = LINE ( 'NONE', #9689, #6147 ) ;
#9603 = CARTESIAN_POINT ( 'NONE',  ( -0.6810530063608482010, -4.461079733298037198, -3.298443181296194293 ) ) ;
#9604 = CARTESIAN_POINT ( 'NONE',  ( 27.93049598394382116, -4.671775696577297410, -3.627061608673664672 ) ) ;
#9605 = AXIS2_PLACEMENT_3D ( 'NONE', #5931, #11455, #10097 ) ;
#9606 = AXIS2_PLACEMENT_3D ( 'NONE', #11685, #7888, #10504 ) ;
#9607 = ORIENTED_EDGE ( 'NONE', *, *, #7188, .T. ) ;
#9608 = B_SPLINE_CURVE_WITH_KNOTS ( 'NONE', 3,
 ( #12078, #17664, #6911, #12174, #14902, #5186 ),
 .UNSPECIFIED., .F., .F.,
 ( 4, 2, 4 ),
 ( 0.000000000000000000, 0.0002095117440854733651, 0.0004190234881709467302 ),
 .UNSPECIFIED. ) ;
#9609 = CARTESIAN_POINT ( 'NONE',  ( 5.500000000000000000, -20.49999999999999645, -6.000000000000000000 ) ) ;
#9610 = CARTESIAN_POINT ( 'NONE',  ( -1.499999999999999778, 9.718191103688258892, -2.333127728361106268 ) ) ;
#9611 = ADVANCED_FACE ( 'NONE', ( #14190 ), #1507, .F. ) ;
#9612 = EDGE_LOOP ( 'NONE', ( #6398, #10236, #15484, #15557, #10446 ) ) ;
#9613 = CARTESIAN_POINT ( 'NONE',  ( 34.25812524399339765, -6.427500325324513319, -5.783357778048663356 ) ) ;
#9614 = ORIENTED_EDGE ( 'NONE', *, *, #3519, .F. ) ;
#9615 = VECTOR ( 'NONE', #12998, 1000.000000000000227 ) ;
#9616 = CARTESIAN_POINT ( 'NONE',  ( 28.91999743871649997, -5.806501378023834370, -3.627061608673668225 ) ) ;
#9617 = CARTESIAN_POINT ( 'NONE',  ( -25.11802603177690330, -16.03270077640482683, 0.5379818257722508434 ) ) ;
#9618 = EDGE_CURVE ( 'NONE', #12431, #15077, #2332, .T. ) ;
#9619 = AXIS2_PLACEMENT_3D ( 'NONE', #1429, #9840, #11013 ) ;
#9620 = ORIENTED_EDGE ( 'NONE', *, *, #12752, .F. ) ;
#9621 = CARTESIAN_POINT ( 'NONE',  ( 32.14213199643172914, -2.910415664685331638, -3.627061608673662896 ) ) ;
#9622 = CARTESIAN_POINT ( 'NONE',  ( 25.71748644841968456, -2.420320648352046078, -5.783357778048663356 ) ) ;
#9623 = CARTESIAN_POINT ( 'NONE',  ( 32.24155699611449677, -1.634298987580965923, -5.783357778048664244 ) ) ;
#9624 = CARTESIAN_POINT ( 'NONE',  ( 27.25621498173240198, -3.499072175709823984, -3.627061608673662008 ) ) ;
#9625 = EDGE_CURVE ( 'NONE', #10340, #1236, #8480, .T. ) ;
#9626 = CARTESIAN_POINT ( 'NONE',  ( 17.40734525178378078, -19.01589366988068974, -15.93907283187074775 ) ) ;
#9627 = ORIENTED_EDGE ( 'NONE', *, *, #11915, .T. ) ;
#9628 = VECTOR ( 'NONE', #12616, 1000.000000000000227 ) ;
#9629 = CARTESIAN_POINT ( 'NONE',  ( 25.76326615456878244, -3.051972493152843580, 4.705209693361168455 ) ) ;
#9630 = CARTESIAN_POINT ( 'NONE',  ( 20.00000000000000000, 7.999999999999996447, 0.000000000000000000 ) ) ;
#9631 = CARTESIAN_POINT ( 'NONE',  ( 16.75000000000000355, -16.63579488892710145, 16.03574476417184158 ) ) ;
#9632 = EDGE_LOOP ( 'NONE', ( #6023, #9669, #7451, #3185 ) ) ;
#9633 = DIRECTION ( 'NONE',  ( 0.000000000000000000, 0.000000000000000000, 1.000000000000000000 ) ) ;
#9634 = ORIENTED_EDGE ( 'NONE', *, *, #14529, .T. ) ;
#9635 = LINE ( 'NONE', #8022, #6654 ) ;
#9636 = VERTEX_POINT ( 'NONE', #7131 ) ;
#9637 = DIRECTION ( 'NONE',  ( 0.000000000000000000, 0.000000000000000000, -1.000000000000000000 ) ) ;
#9638 = CARTESIAN_POINT ( 'NONE',  ( 30.15443244188179150, -1.895953141405084086, -5.783357778048658027 ) ) ;
#9639 = VECTOR ( 'NONE', #10663, 1000.000000000000227 ) ;
#9640 = LINE ( 'NONE', #10900, #5475 ) ;
#9641 = DIRECTION ( 'NONE',  ( 0.000000000000000000, 0.000000000000000000, 1.000000000000000000 ) ) ;
#9642 = DIRECTION ( 'NONE',  ( -0.000000000000000000, -0.000000000000000000, 1.000000000000000000 ) ) ;
#9643 =( BOUNDED_CURVE ( )  B_SPLINE_CURVE ( 2, ( #15298, #16672, #5587, #2880, #7067, #4245, #76, #14538, #14438 ),
 .UNSPECIFIED., .F., .T. ) 
 B_SPLINE_CURVE_WITH_KNOTS ( ( 3, 2, 2, 2, 3 ),
 ( 0.2115384615384615641, 0.2179487179487179516, 0.2307692307692307820, 0.2435897435897435848, 0.2500000000000000000 ),
 .UNSPECIFIED. ) 
 CURVE ( )  GEOMETRIC_REPRESENTATION_ITEM ( )  RATIONAL_B_SPLINE_CURVE ( ( 0.9330127018922194093, 0.9330127018922196314, 1.000000000000000000, 0.8660254037844387076, 1.000000000000000000, 0.8660254037844387076, 1.000000000000000000, 0.9330127018922191873, 0.9330127018922194093 ) ) 
 REPRESENTATION_ITEM ( '' )  );
#9644 = CARTESIAN_POINT ( 'NONE',  ( 29.62489513447700062, -6.348545659133139729, 4.705209693361160461 ) ) ;
#9645 = EDGE_CURVE ( 'NONE', #1319, #3307, #9913, .T. ) ;
#9646 = DIRECTION ( 'NONE',  ( -0.9979201627913403261, 0.06446199418653535129, 0.000000000000000000 ) ) ;
#9647 = DIRECTION ( 'NONE',  ( 0.000000000000000000, 0.000000000000000000, -1.000000000000000000 ) ) ;
#9648 = ORIENTED_EDGE ( 'NONE', *, *, #9524, .T. ) ;
#9649 = VERTEX_POINT ( 'NONE', #9818 ) ;
#9650 = CARTESIAN_POINT ( 'NONE',  ( 26.84461768998868436, -2.294720455324902542, 5.783357778048668685 ) ) ;
#9651 = DIRECTION ( 'NONE',  ( -0.000000000000000000, -1.000000000000000000, -0.000000000000000000 ) ) ;
#9652 = EDGE_LOOP ( 'NONE', ( #7518, #6777, #5900, #13705 ) ) ;
#9653 = CARTESIAN_POINT ( 'NONE',  ( 27.65458886993626564, -2.824105456627233224, 4.705209693361168455 ) ) ;
#9654 = CARTESIAN_POINT ( 'NONE',  ( 31.24221605398236079, -5.726592414339752857, -8.283357778048664244 ) ) ;
#9655 = LINE ( 'NONE', #13673, #4031 ) ;
#9656 = CARTESIAN_POINT ( 'NONE',  ( 31.34233605952372415, -6.778795339760710803, 5.783357778048664244 ) ) ;
#9657 = DIRECTION ( 'NONE',  ( -5.026720092345836698E-22, 4.581671729415424240E-22, -1.000000000000000000 ) ) ;
#9658 = DIRECTION ( 'NONE',  ( 0.000000000000000000, 0.000000000000000000, 1.000000000000000000 ) ) ;
#9659 = CARTESIAN_POINT ( 'NONE',  ( 28.99436501219896201, -4.543600488427916417, -3.283357778048664688 ) ) ;
#9660 = DIRECTION ( 'NONE',  ( 0.000000000000000000, 0.000000000000000000, -1.000000000000000000 ) ) ;
#9661 = FACE_OUTER_BOUND ( 'NONE', #15199, .T. ) ;
#9662 = CARTESIAN_POINT ( 'NONE',  ( 27.69360539047986336, -12.07076363665953345, 13.80168160306295810 ) ) ;
#9663 =( LENGTH_UNIT ( ) NAMED_UNIT ( * ) SI_UNIT ( .MILLI., .METRE. ) );
#9664 = ORIENTED_EDGE ( 'NONE', *, *, #16624, .T. ) ;
#9665 =( BOUNDED_CURVE ( )  B_SPLINE_CURVE ( 2, ( #7082, #15412, #9951, #13783, #15502, #14137, #2998, #11402, #4346 ),
 .UNSPECIFIED., .F., .T. ) 
 B_SPLINE_CURVE_WITH_KNOTS ( ( 3, 2, 2, 2, 3 ),
 ( 0.05769230769230771633, 0.06410256410256409687, 0.07692307692307692735, 0.08974358974358974395, 0.09615384615384617306 ),
 .UNSPECIFIED. ) 
 CURVE ( )  GEOMETRIC_REPRESENTATION_ITEM ( )  RATIONAL_B_SPLINE_CURVE ( ( 0.9330127018922194093, 0.9330127018922196314, 1.000000000000000000, 0.8660254037844387076, 1.000000000000000000, 0.8660254037844387076, 1.000000000000000000, 0.9330127018922191873, 0.9330127018922194093 ) ) 
 REPRESENTATION_ITEM ( '' )  );
#9666 = EDGE_CURVE ( 'NONE', #11972, #714, #2054, .T. ) ;
#9667 = CARTESIAN_POINT ( 'NONE',  ( 28.89355063163679915, -2.047864499088824175, -5.783357778048658027 ) ) ;
#9668 = CARTESIAN_POINT ( 'NONE',  ( 28.91999743871649997, -5.806501378023834370, -3.627061608673668225 ) ) ;
#9669 = ORIENTED_EDGE ( 'NONE', *, *, #6725, .T. ) ;
#9670 = CYLINDRICAL_SURFACE ( 'NONE', #12112, 5.000000000000001776 ) ;
#9671 = CARTESIAN_POINT ( 'NONE',  ( 31.89397184978405519, -6.712334120981523711, -5.783357778048663356 ) ) ;
#9672 = EDGE_LOOP ( 'NONE', ( #13955, #12949, #1315, #10879, #13886 ) ) ;
#9673 = ORIENTED_EDGE ( 'NONE', *, *, #7981, .F. ) ;
#9674 = CARTESIAN_POINT ( 'NONE',  ( 31.49429780130001788, -5.496349022752856861, 3.627061608673662896 ) ) ;
#9675 = CARTESIAN_POINT ( 'NONE',  ( 29.41022140756759029, -3.239556939666760726, -7.939653947423660263 ) ) ;
#9676 = LINE ( 'NONE', #15227, #7486 ) ;
#9677 = CARTESIAN_POINT ( 'NONE',  ( -5.499998817156067865, -20.49639288455253450, -12.00000000000000000 ) ) ;
#9678 = LINE ( 'NONE', #13865, #6996 ) ;
#9679 = CARTESIAN_POINT ( 'NONE',  ( 27.93049598394382116, -4.671775696577297410, -3.627061608673664672 ) ) ;
#9680 = DIRECTION ( 'NONE',  ( 0.000000000000000000, 0.000000000000000000, 1.000000000000000000 ) ) ;
#9681 = DIRECTION ( 'NONE',  ( -1.000000000000000000, 0.000000000000000000, 0.000000000000000000 ) ) ;
#9682 = LINE ( 'NONE', #12334, #2949 ) ;
#9683 = CARTESIAN_POINT ( 'NONE',  ( 29.35089333861488115, -5.954459450865362768, -8.283357778048662468 ) ) ;
#9684 = ORIENTED_EDGE ( 'NONE', *, *, #16011, .F. ) ;
#9685 = ORIENTED_EDGE ( 'NONE', *, *, #3693, .F. ) ;
#9686 = CARTESIAN_POINT ( 'NONE',  ( 30.64918316926811315, -2.463315982128351678, -6.861505862736159145 ) ) ;
#9687 = DIRECTION ( 'NONE',  ( 0.1196152422706605323, -0.9928203230275512992, 0.000000000000000000 ) ) ;
#9688 = FACE_OUTER_BOUND ( 'NONE', #13430, .T. ) ;
#9689 = CARTESIAN_POINT ( 'NONE',  ( -15.92260893619738837, -28.39189527176317540, -12.00000000000000000 ) ) ;
#9690 = CARTESIAN_POINT ( 'NONE',  ( 8.874038404635971489, 3.391377654146752629, -2.000000000000000000 ) ) ;
#9691 = EDGE_CURVE ( 'NONE', #5666, #17327, #3191, .T. ) ;
#9692 = CARTESIAN_POINT ( 'NONE',  ( 29.36638131047866906, -1.990897739957422807, -5.783357778048658915 ) ) ;
#9693 = VERTEX_POINT ( 'NONE', #4570 ) ;
#9694 = ADVANCED_FACE ( 'NONE', ( #5742 ), #15544, .F. ) ;
#9695 = CARTESIAN_POINT ( 'NONE',  ( 0.000000000000000000, 0.000000000000000000, -3.000000000000000000 ) ) ;
#9696 = DIRECTION ( 'NONE',  ( 1.000000000000000000, 0.000000000000000000, 0.000000000000000000 ) ) ;
#9697 = ORIENTED_EDGE ( 'NONE', *, *, #15992, .F. ) ;
#9698 = DIRECTION ( 'NONE',  ( -0.000000000000000000, 1.000000000000000000, -3.469446951953614189E-16 ) ) ;
#9699 = ORIENTED_EDGE ( 'NONE', *, *, #14498, .T. ) ;
#9700 = CARTESIAN_POINT ( 'NONE',  ( 31.67382807612511542, -6.101689702897060030, -6.861505862736167138 ) ) ;
#9701 = FACE_OUTER_BOUND ( 'NONE', #4269, .T. ) ;
#9702 = VERTEX_POINT ( 'NONE', #15461 ) ;
#9703 = CARTESIAN_POINT ( 'NONE',  ( 31.71314141467879111, -4.216041623526076698, -3.627061608673664672 ) ) ;
#9704 = DIRECTION ( 'NONE',  ( 1.000000000000000000, 0.000000000000000000, 0.000000000000000000 ) ) ;
#9705 = DIRECTION ( 'NONE',  ( 1.000000000000000000, 0.000000000000000000, 0.000000000000000000 ) ) ;
#9706 = CARTESIAN_POINT ( 'NONE',  ( 26.63030083514515312, -6.709335133632020387, -6.861505862736167138 ) ) ;
#9707 = EDGE_CURVE ( 'NONE', #13014, #8806, #594, .T. ) ;
#9708 = EDGE_LOOP ( 'NONE', ( #15937, #11850 ) ) ;
#9709 = LINE ( 'NONE', #1583, #5408 ) ;
#9710 = ORIENTED_EDGE ( 'NONE', *, *, #17001, .F. ) ;
#9711 = ORIENTED_EDGE ( 'NONE', *, *, #4119, .F. ) ;
#9712 = EDGE_CURVE ( 'NONE', #11061, #14045, #8105, .T. ) ;
#9713 = CARTESIAN_POINT ( 'NONE',  ( 9.480241546517731877, -0.6123889447720862744, -6.899999999999998579 ) ) ;
#9714 = CARTESIAN_POINT ( 'NONE',  ( 33.09223089549517738, -4.049888575955752579, 3.283357778048664244 ) ) ;
#9715 = EDGE_LOOP ( 'NONE', ( #17012, #2716, #13777, #11532, #9921, #17006, #2846, #8307, #6259, #2710, #5068, #6354, #15112, #7193, #15398, #4671, #9224, #5556, #3539, #17788, #15524, #8712, #10718, #9394, #454, #8921, #9369, #13037, #13764 ) ) ;
#9716 = VERTEX_POINT ( 'NONE', #11540 ) ;
#9717 = CARTESIAN_POINT ( 'NONE',  ( 26.01652455409633902, -4.902371455920928156, -5.783357778048663356 ) ) ;
#9718 = PLANE ( 'NONE',  #6734 ) ;
#9719 = CARTESIAN_POINT ( 'NONE',  ( 27.77288575766320378, -4.690764616287755651, -7.939653947423662039 ) ) ;
#9720 = CARTESIAN_POINT ( 'NONE',  ( 45.00000000000000711, 0.000000000000000000, -5.537981825772250843 ) ) ;
#9721 = CARTESIAN_POINT ( 'NONE',  ( 29.69163902039066372, -1.941513746749485847, 5.113484796970859669 ) ) ;
#9722 = DIRECTION ( 'NONE',  ( -1.000000000000000000, 0.000000000000000000, 0.000000000000000000 ) ) ;
#9723 = CARTESIAN_POINT ( 'NONE',  ( 0.000000000000000000, 0.000000000000000000, -10.50000000000000000 ) ) ;
#9724 = CIRCLE ( 'NONE', #1949, 6.249999999999998224 ) ;
#9725 = CARTESIAN_POINT ( 'NONE',  ( 28.38593337277646711, -7.124786616671554107, 5.783357778048658027 ) ) ;
#9726 = CARTESIAN_POINT ( 'NONE',  ( 45.50000000000000000, -16.03270077640482683, 8.287981825772238409 ) ) ;
#9727 = DIRECTION ( 'NONE',  ( 0.000000000000000000, 0.000000000000000000, -1.000000000000000000 ) ) ;
#9728 = DIRECTION ( 'NONE',  ( -1.000000000000000000, 0.000000000000000000, 0.000000000000000000 ) ) ;
#9729 = EDGE_LOOP ( 'NONE', ( #17051, #11759 ) ) ;
#9730 = ORIENTED_EDGE ( 'NONE', *, *, #16806, .T. ) ;
#9731 = CARTESIAN_POINT ( 'NONE',  ( 27.72904566057427189, -3.442105416578422172, 7.939653947423664704 ) ) ;
#9732 = CARTESIAN_POINT ( 'NONE',  ( 26.73899421642883567, -2.634607751922174224, 7.033357778048666020 ) ) ;
#9733 = ORIENTED_EDGE ( 'NONE', *, *, #3475, .F. ) ;
#9734 = CARTESIAN_POINT ( 'NONE',  ( 27.25621498173240198, -3.499072175709823984, 7.939653947423662927 ) ) ;
#9735 = VERTEX_POINT ( 'NONE', #1685 ) ;
#9736 = ORIENTED_EDGE ( 'NONE', *, *, #4639, .T. ) ;
#9737 = FACE_OUTER_BOUND ( 'NONE', #17462, .T. ) ;
#9738 = DIRECTION ( 'NONE',  ( -0.1196152422706611984, 0.9928203230275510771, 0.000000000000000000 ) ) ;
#9739 = EDGE_CURVE ( 'NONE', #364, #2889, #8434, .T. ) ;
#9740 = CARTESIAN_POINT ( 'NONE',  ( 28.53771668024168662, -2.080538600569502794, 5.783357778048667797 ) ) ;
#9741 = CARTESIAN_POINT ( 'NONE',  ( 25.74134610602432360, -2.427642893298174620, -5.783357778048658027 ) ) ;
#9742 = CARTESIAN_POINT ( 'NONE',  ( 26.16860980394290337, -3.430234601869349920, -3.283357778048662023 ) ) ;
#9743 =( BOUNDED_CURVE ( )  B_SPLINE_CURVE ( 2, ( #650, #11877, #2114, #17360, #15982, #6174, #3724, #11697, #17266 ),
 .UNSPECIFIED., .F., .T. ) 
 B_SPLINE_CURVE_WITH_KNOTS ( ( 3, 2, 2, 2, 3 ),
 ( 0.5576923076923077094, 0.5641025641025640969, 0.5769230769230768718, 0.5897435897435897578, 0.5961538461538461453 ),
 .UNSPECIFIED. ) 
 CURVE ( )  GEOMETRIC_REPRESENTATION_ITEM ( )  RATIONAL_B_SPLINE_CURVE ( ( 0.9330127018922194093, 0.9330127018922194093, 1.000000000000000000, 0.8660254037844387076, 1.000000000000000000, 0.8660254037844387076, 1.000000000000000000, 0.9330127018922194093, 0.9330127018922194093 ) ) 
 REPRESENTATION_ITEM ( '' )  );
#9744 = CARTESIAN_POINT ( 'NONE',  ( 28.83304567166618781, -6.743756660494150346, -7.033357778048666908 ) ) ;
#9745 = DIRECTION ( 'NONE',  ( 0.000000000000000000, 0.000000000000000000, 1.000000000000000000 ) ) ;
#9746 = VECTOR ( 'NONE', #3854, 1000.000000000000000 ) ;
#9747 = CARTESIAN_POINT ( 'NONE',  ( 23.84286890107044954, -10.01213378893004879, -14.74186762137086859 ) ) ;
#9748 = CARTESIAN_POINT ( 'NONE',  ( 26.31556265977298992, -7.384422263489805793, 5.783357778048663356 ) ) ;
#9749 =( NAMED_UNIT ( * ) SI_UNIT ( $, .STERADIAN. ) SOLID_ANGLE_UNIT ( ) );
#9750 = CARTESIAN_POINT ( 'NONE',  ( 32.34358231980129261, -4.140085944684206432, -3.627061608673664672 ) ) ;
#9751 = ORIENTED_EDGE ( 'NONE', *, *, #985, .F. ) ;
#9752 = CARTESIAN_POINT ( 'NONE',  ( 29.65098506949083301, -2.583579140294649523, -4.705209693361160461 ) ) ;
#9753 = CYLINDRICAL_SURFACE ( 'NONE', #7806, 10.50000000000000000 ) ;
#9754 = VERTEX_POINT ( 'NONE', #15641 ) ;
#9755 = ORIENTED_EDGE ( 'NONE', *, *, #6976, .T. ) ;
#9756 = ORIENTED_EDGE ( 'NONE', *, *, #528, .T. ) ;
#9757 = CARTESIAN_POINT ( 'NONE',  ( 28.14933959732260149, -3.391468297350500372, 3.627061608673666449 ) ) ;
#9758 = CARTESIAN_POINT ( 'NONE',  ( 31.80137159822941939, -6.386132006154467078, 7.033357778048657138 ) ) ;
#9759 = DIRECTION ( 'NONE',  ( 0.000000000000000000, 0.000000000000000000, 1.000000000000000000 ) ) ;
#9760 = CARTESIAN_POINT ( 'NONE',  ( 25.75741033704265703, -2.751693534003876174, -5.973512092880350011 ) ) ;
#9761 = CARTESIAN_POINT ( 'NONE',  ( 20.00000000000000000, 7.999999999999996447, -15.51150668642334374 ) ) ;
#9762 = CARTESIAN_POINT ( 'NONE',  ( 30.25080928106424594, -3.138282701210941994, -3.627061608673662896 ) ) ;
#9763 = CARTESIAN_POINT ( 'NONE',  ( -2.000000000000002220, 3.464101615137751278, 0.000000000000000000 ) ) ;
#9764 = EDGE_CURVE ( 'NONE', #3060, #15522, #11871, .T. ) ;
#9765 = DIRECTION ( 'NONE',  ( 0.9928203230275511881, 0.1196152422706610180, 9.614813431917825245E-17 ) ) ;
#9766 = VERTEX_POINT ( 'NONE', #1877 ) ;
#9767 = VECTOR ( 'NONE', #5326, 1000.000000000000227 ) ;
#9768 = CARTESIAN_POINT ( 'NONE',  ( 36.27615609941022257, -23.17738945083361557, -12.00000000000000000 ) ) ;
#9769 =( BOUNDED_CURVE ( )  B_SPLINE_CURVE ( 2, ( #13587, #5228, #6782, #17708, #3804, #1168, #9320, #10578, #7790 ),
 .UNSPECIFIED., .F., .T. ) 
 B_SPLINE_CURVE_WITH_KNOTS ( ( 3, 2, 2, 2, 3 ),
 ( 0.4423076923076923461, 0.4487179487179487336, 0.4615384615384615641, 0.4743589743589743390, 0.4807692307692307820 ),
 .UNSPECIFIED. ) 
 CURVE ( )  GEOMETRIC_REPRESENTATION_ITEM ( )  RATIONAL_B_SPLINE_CURVE ( ( 0.9330127018922194093, 0.9330127018922196314, 1.000000000000000000, 0.8660254037844387076, 1.000000000000000000, 0.8660254037844387076, 1.000000000000000000, 0.9330127018922190762, 0.9330127018922194093 ) ) 
 REPRESENTATION_ITEM ( '' )  );
#9770 = CARTESIAN_POINT ( 'NONE',  ( 28.15758777499317489, -7.552042790248305160, -5.783357778048669573 ) ) ;
#9771 = CARTESIAN_POINT ( 'NONE',  ( 30.88577694472199298, -6.196634301449400084, -6.861505862736166250 ) ) ;
#9772 = VECTOR ( 'NONE', #16741, 1000.000000000000000 ) ;
#9773 = FACE_OUTER_BOUND ( 'NONE', #4000, .T. ) ;
#9774 = CARTESIAN_POINT ( 'NONE',  ( 14.00000000000000178, 1.714505518806294835E-15, -10.50000000000000000 ) ) ;
#9775 = CARTESIAN_POINT ( 'NONE',  ( 0.000000000000000000, 0.000000000000000000, -8.722503561260788629 ) ) ;
#9776 = CARTESIAN_POINT ( 'NONE',  ( 30.35023428074701002, -1.862166024106576057, -5.783357778048664244 ) ) ;
#9777 = CARTESIAN_POINT ( 'NONE',  ( 31.70371634254663817, -2.036456781249897485, 7.033357778048666020 ) ) ;
#9778 = CARTESIAN_POINT ( 'NONE',  ( 29.99682221560115991, -1.914942061115552541, -5.783357778048658915 ) ) ;
#9779 = AXIS2_PLACEMENT_3D ( 'NONE', #359, #8322, #2987 ) ;
#9780 = ORIENTED_EDGE ( 'NONE', *, *, #11689, .F. ) ;
#9781 = ORIENTED_EDGE ( 'NONE', *, *, #10733, .F. ) ;
#9782 = CARTESIAN_POINT ( 'NONE',  ( 26.85044460880409645, -7.319979551716484067, 5.783357778048657138 ) ) ;
#9783 = CARTESIAN_POINT ( 'NONE',  ( 30.54048978798443059, -6.538043363838207611, -4.533357778048668685 ) ) ;
#9784 = ADVANCED_FACE ( 'NONE', ( #7406 ), #6014, .F. ) ;
#9785 = DIRECTION ( 'NONE',  ( 0.000000000000000000, 1.000000000000000000, 0.000000000000000000 ) ) ;
#9786 = ORIENTED_EDGE ( 'NONE', *, *, #2827, .F. ) ;
#9787 = EDGE_CURVE ( 'NONE', #5445, #15456, #15740, .T. ) ;
#9788 = CARTESIAN_POINT ( 'NONE',  ( 30.82871344409320713, -3.068656662272551294, -7.939653947423660263 ) ) ;
#9789 = DIRECTION ( 'NONE',  ( -1.000000000000000000, -0.000000000000000000, -0.000000000000000000 ) ) ;
#9790 = CIRCLE ( 'NONE', #9245, 2.100000000000000089 ) ;
#9791 = VERTEX_POINT ( 'NONE', #3398 ) ;
#9792 = VERTEX_POINT ( 'NONE', #17208 ) ;
#9793 = CARTESIAN_POINT ( 'NONE',  ( 30.04066231269008469, -3.163601260824890904, -7.939653947423660263 ) ) ;
#9794 = ADVANCED_FACE ( 'NONE', ( #13191 ), #855, .T. ) ;
#9795 = LINE ( 'NONE', #16534, #9528 ) ;
#9796 = CARTESIAN_POINT ( 'NONE',  ( 4.197478771013683385, -0.8523759490158154817, -3.205061274276559846 ) ) ;
#9797 = ORIENTED_EDGE ( 'NONE', *, *, #14891, .T. ) ;
#9798 = CARTESIAN_POINT ( 'NONE',  ( 32.89331279191618762, -2.620040694222726785, -8.283357778048658915 ) ) ;
#9799 = CIRCLE ( 'NONE', #5457, 10.50000000000000000 ) ;
#9800 = VERTEX_POINT ( 'NONE', #3758 ) ;
#9801 = CARTESIAN_POINT ( 'NONE',  ( 16.75000000000000355, -16.63579488892710145, -16.03574476417184158 ) ) ;
#9802 = ORIENTED_EDGE ( 'NONE', *, *, #12695, .F. ) ;
#9803 = CARTESIAN_POINT ( 'NONE',  ( 29.94002636988270538, -4.429666970165102136, 3.283357778048664244 ) ) ;
#9804 = AXIS2_PLACEMENT_3D ( 'NONE', #10644, #6231, #7866 ) ;
#9805 = DIRECTION ( 'NONE',  ( 1.000000000000000000, 0.000000000000000000, 0.000000000000000000 ) ) ;
#9806 =( NAMED_UNIT ( * ) SI_UNIT ( $, .STERADIAN. ) SOLID_ANGLE_UNIT ( ) );
#9807 = CARTESIAN_POINT ( 'NONE',  ( 33.78529456515154550, -6.484467084455913799, -5.783357778048663356 ) ) ;
#9808 = VERTEX_POINT ( 'NONE', #14737 ) ;
#9809 = FACE_OUTER_BOUND ( 'NONE', #10517, .T. ) ;
#9810 = ORIENTED_EDGE ( 'NONE', *, *, #5877, .T. ) ;
#9811 = VECTOR ( 'NONE', #9150, 1000.000000000000114 ) ;
#9812 = CARTESIAN_POINT ( 'NONE',  ( 26.64639396487419987, -2.308405637095112706, 5.783357778048667797 ) ) ;
#9813 = ADVANCED_FACE ( 'NONE', ( #2051 ), #7746, .T. ) ;
#9814 = ORIENTED_EDGE ( 'NONE', *, *, #17303, .F. ) ;
#9815 = DIRECTION ( 'NONE',  ( -0.000000000000000000, -0.000000000000000000, 1.000000000000000000 ) ) ;
#9816 = CARTESIAN_POINT ( 'NONE',  ( 27.86926259684567597, -5.933094176093606897, -7.939653947423664704 ) ) ;
#9817 = CARTESIAN_POINT ( 'NONE',  ( 32.27410075503257758, -1.240829931302721345, -5.783357778048658027 ) ) ;
#9818 = CARTESIAN_POINT ( 'NONE',  ( 28.45891156537951971, -2.090033060632186412, 5.783357778048657138 ) ) ;
#9819 = DIRECTION ( 'NONE',  ( -0.8660254037844432595, -0.4999999999999921174, 0.000000000000000000 ) ) ;
#9820 = EDGE_CURVE ( 'NONE', #3773, #12766, #14489, .T. ) ;
#9821 = CARTESIAN_POINT ( 'NONE',  ( 32.32618902979206865, -6.650063623909865385, -5.783357778048669573 ) ) ;
#9822 = CYLINDRICAL_SURFACE ( 'NONE', #8758, 2.749999999999992006 ) ;
#9823 = CARTESIAN_POINT ( 'NONE',  ( 30.42903939560917337, -1.852671564043892660, -5.783357778048658027 ) ) ;
#9824 = CARTESIAN_POINT ( 'NONE',  ( 31.54230778485832332, -2.355712103769039611, 6.861505862736166250 ) ) ;
#9825 = CIRCLE ( 'NONE', #15049, 6.000000000000000888 ) ;
#9826 = VERTEX_POINT ( 'NONE', #11726 ) ;
#9827 = B_SPLINE_CURVE_WITH_KNOTS ( 'NONE', 3,
 ( #7448, #5700, #12968, #553, #469, #11217 ),
 .UNSPECIFIED., .F., .F.,
 ( 4, 2, 4 ),
 ( 0.002452478801916362864, 0.003676905084147999610, 0.004901331366379636789 ),
 .UNSPECIFIED. ) ;
#9828 = EDGE_LOOP ( 'NONE', ( #5204, #16869, #17131, #3018, #11335, #17853 ) ) ;
#9829 = ORIENTED_EDGE ( 'NONE', *, *, #13419, .T. ) ;
#9830 = CARTESIAN_POINT ( 'NONE',  ( 29.36638131047866196, -1.990897739957422807, 5.783357778048668685 ) ) ;
#9831 = SURFACE_STYLE_USAGE ( .BOTH. , #5849 ) ;
#9832 = DIRECTION ( 'NONE',  ( 0.9979201627913403261, -0.06446199418653547619, 0.000000000000000000 ) ) ;
#9833 = VECTOR ( 'NONE', #221, 1000.000000000000227 ) ;
#9834 = ORIENTED_EDGE ( 'NONE', *, *, #14225, .T. ) ;
#9835 = CARTESIAN_POINT ( 'NONE',  ( 30.42903939560917337, -1.852671564043892660, 5.783357778048667797 ) ) ;
#9836 = LINE ( 'NONE', #4415, #10078 ) ;
#9837 = DIRECTION ( 'NONE',  ( 0.6287809056569716448, 0.6925565483635240938, -0.3535533905932743415 ) ) ;
#9838 = EDGE_CURVE ( 'NONE', #14231, #7158, #2620, .T. ) ;
#9839 = CARTESIAN_POINT ( 'NONE',  ( -9.500000000000001776, 0.000000000000000000, -2.000000000000000000 ) ) ;
#9840 = DIRECTION ( 'NONE',  ( -1.000000000000000000, 0.000000000000000000, 0.000000000000000000 ) ) ;
#9841 = CARTESIAN_POINT ( 'NONE',  ( -30.05650519998691195, -5.408673599982547486, -13.28483438372753156 ) ) ;
#9842 = CARTESIAN_POINT ( 'NONE',  ( 30.57046727500519978, -4.353711291323232757, -8.283357778048662468 ) ) ;
#9843 = CARTESIAN_POINT ( 'NONE',  ( -3.248936832696171617, -15.16081378324841111, 17.00000000000000000 ) ) ;
#9844 = CARTESIAN_POINT ( 'NONE',  ( -2.100000000000000089, 2.571758278209441957E-16, -4.700000000000000178 ) ) ;
#9845 = CARTESIAN_POINT ( 'NONE',  ( 30.86385689617752348, -5.572304701594726239, -7.939653947423664704 ) ) ;
#9846 = ORIENTED_EDGE ( 'NONE', *, *, #4147, .F. ) ;
#9847 = CARTESIAN_POINT ( 'NONE',  ( 25.90419076669538256, -3.969988049114259177, -7.913474645583921330 ) ) ;
#9848 = VECTOR ( 'NONE', #4450, 1000.000000000000000 ) ;
#9849 = DIRECTION ( 'NONE',  ( 0.000000000000000000, -1.000000000000000000, 0.000000000000000000 ) ) ;
#9850 = EDGE_CURVE ( 'NONE', #5034, #16160, #10542, .T. ) ;
#9851 = ORIENTED_EDGE ( 'NONE', *, *, #12669, .F. ) ;
#9852 = ORIENTED_EDGE ( 'NONE', *, *, #5421, .F. ) ;
#9853 = CARTESIAN_POINT ( 'NONE',  ( 30.12381574833269937, -2.526612381163247267, 6.861505862736165362 ) ) ;
#9854 = CARTESIAN_POINT ( 'NONE',  ( 26.99805802979993885, -6.665027654307603022, -4.705209693361168455 ) ) ;
#9855 = DIRECTION ( 'NONE',  ( 0.000000000000000000, 0.000000000000000000, 1.000000000000000000 ) ) ;
#9856 = LINE ( 'NONE', #6979, #575 ) ;
#9857 = CYLINDRICAL_SURFACE ( 'NONE', #14818, 2.500000000000001776 ) ;
#9859 = VECTOR ( 'NONE', #12149, 1000.000000000000227 ) ;
#9858 = CARTESIAN_POINT ( 'NONE',  ( 28.77978050244509944, -3.315512618508630993, -7.939653947423660263 ) ) ;
#9860 = CARTESIAN_POINT ( 'NONE',  ( 31.95146207396702565, -5.641142275435199416, -8.283357778048664244 ) ) ;
#9861 = CARTESIAN_POINT ( 'NONE',  ( 26.01652455409633902, -4.902371455920926380, 5.783357778048663356 ) ) ;
#9862 = CIRCLE ( 'NONE', #3813, 5.000000000000000000 ) ;
#9863 = CARTESIAN_POINT ( 'NONE',  ( 2.000000000000002665, -3.464101615137751278, 0.000000000000000000 ) ) ;
#9864 = CARTESIAN_POINT ( 'NONE',  ( 28.05993251931039012, -3.202367565343739564, -3.283357778048662023 ) ) ;
#9865 = VECTOR ( 'NONE', #12511, 1000.000000000000000 ) ;
#9866 = ORIENTED_EDGE ( 'NONE', *, *, #8844, .F. ) ;
#9867 = CARTESIAN_POINT ( 'NONE',  ( 28.75786045390062995, -2.691183018653962034, -6.861505862736159145 ) ) ;
#9868 = CARTESIAN_POINT ( 'NONE',  ( 25.29083129957448151, -4.989803161779970964, 5.783357778048662468 ) ) ;
#9869 = CARTESIAN_POINT ( 'NONE',  ( 32.95080301609915097, -1.548848848676412260, 5.783357778048663356 ) ) ;
#9870 = CARTESIAN_POINT ( 'NONE',  ( 28.71361296893772774, -7.095504558991913235, 6.453230759126468818 ) ) ;
#9871 = ADVANCED_FACE ( 'NONE', ( #4926 ), #10456, .F. ) ;
#9872 = CARTESIAN_POINT ( 'NONE',  ( 30.64556327217151122, -6.525384084031224496, 4.533357778048659803 ) ) ;
#9873 = CARTESIAN_POINT ( 'NONE',  ( 30.01874226414561875, -2.539271660970221944, -6.861505862736159145 ) ) ;
#9874 = AXIS2_PLACEMENT_3D ( 'NONE', #2227, #10538, #17290 ) ;
#9875 = AXIS2_PLACEMENT_3D ( 'NONE', #2556, #10779, #9260 ) ;
#9876 = ORIENTED_EDGE ( 'NONE', *, *, #2277, .T. ) ;
#9877 = ORIENTED_EDGE ( 'NONE', *, *, #6385, .T. ) ;
#9878 = CIRCLE ( 'NONE', #3238, 2.500000000000001776 ) ;
#9879 = CARTESIAN_POINT ( 'NONE',  ( -12.50000000000000000, 0.000000000000000000, -4.000000000000000000 ) ) ;
#9880 = DIRECTION ( 'NONE',  ( 0.000000000000000000, 0.000000000000000000, -1.000000000000000000 ) ) ;
#9881 = AXIS2_PLACEMENT_3D ( 'NONE', #6712, #13612, #16512 ) ;
#9882 = CARTESIAN_POINT ( 'NONE',  ( -23.43428999263575818, -9.970190943884908563, -14.83168556311182940 ) ) ;
#9883 = EDGE_CURVE ( 'NONE', #11770, #5221, #8982, .T. ) ;
#9884 = EDGE_LOOP ( 'NONE', ( #6305, #10370, #7930, #17787 ) ) ;
#9885 = PRODUCT_RELATED_PRODUCT_CATEGORY ( 'part', '', ( #2317 ) ) ;
#9886 = FACE_OUTER_BOUND ( 'NONE', #5919, .T. ) ;
#9887 = CIRCLE ( 'NONE', #11932, 9.500000000000001776 ) ;
#9888 = EDGE_LOOP ( 'NONE', ( #2288, #6255, #13536, #8728 ) ) ;
#9889 = CARTESIAN_POINT ( 'NONE',  ( 30.25080928106424594, -3.138282701210941994, -3.627061608673662896 ) ) ;
#9890 = VECTOR ( 'NONE', #4936, 1000.000000000000000 ) ;
#9891 = CARTESIAN_POINT ( 'NONE',  ( 26.01652455409633902, -4.902371455920928156, -5.783357778048663356 ) ) ;
#9892 = CARTESIAN_POINT ( 'NONE',  ( 0.000000000000000000, 0.000000000000000000, -3.000000000000002665 ) ) ;
#9893 = CARTESIAN_POINT ( 'NONE',  ( 32.85952466860454280, -1.897204703373130741, -7.033357778048658027 ) ) ;
#9894 = CIRCLE ( 'NONE', #5267, 12.50000000000000000 ) ;
#9895 = CARTESIAN_POINT ( 'NONE',  ( 29.54600080245929306, -4.477139269648729325, -3.283357778048664688 ) ) ;
#9896 = EDGE_LOOP ( 'NONE', ( #13852, #8514, #17613, #16402 ) ) ;
#9897 = CARTESIAN_POINT ( 'NONE',  ( 26.00347982711925710, -2.723222710571018279, 4.533357778048667797 ) ) ;
#9898 = CONICAL_SURFACE ( 'NONE', #12530, 3.425051884552432480, 0.7853981633974544962 ) ;
#9899 = AXIS2_PLACEMENT_3D ( 'NONE', #1955, #15732, #8752 ) ;
#9900 = CARTESIAN_POINT ( 'NONE',  ( 26.37178701114681800, -2.351687214456304353, 5.783357778048668685 ) ) ;
#9901 = CARTESIAN_POINT ( 'NONE',  ( -28.59532824046058153, -19.01044845393195715, 13.55637998813296186 ) ) ;
#9902 = DIRECTION ( 'NONE',  ( -0.000000000000000000, -0.000000000000000000, -1.000000000000000000 ) ) ;
#9903 = EDGE_LOOP ( 'NONE', ( #5003, #5072 ) ) ;
#9904 = VECTOR ( 'NONE', #16465, 1000.000000000000227 ) ;
#9905 = SURFACE_STYLE_USAGE ( .BOTH. , #15453 ) ;
#9906 = EDGE_LOOP ( 'NONE', ( #1402, #12792, #17047, #11782 ) ) ;
#9907 = DIRECTION ( 'NONE',  ( -1.000000000000000000, 0.000000000000000000, 0.000000000000000000 ) ) ;
#9908 = ORIENTED_EDGE ( 'NONE', *, *, #13392, .T. ) ;
#9909 = CARTESIAN_POINT ( 'NONE',  ( 27.53153627355490229, -7.237921456612971483, -5.113484796970862334 ) ) ;
#9910 = CARTESIAN_POINT ( 'NONE',  ( 27.12922144900085186, -2.887401855662130146, -4.705209693361160461 ) ) ;
#9911 = CARTESIAN_POINT ( 'NONE',  ( 31.32102116884452414, -5.717097954277069682, -8.283357778048662468 ) ) ;
#9912 = TOROIDAL_SURFACE ( 'NONE', #8790, 10.40000000000000036, 0.9000000000000003553 ) ;
#9913 = LINE ( 'NONE', #14016, #5776 ) ;
#9914 = SHAPE_DEFINITION_REPRESENTATION ( #9247, #5639 ) ;
#9915 = CARTESIAN_POINT ( 'NONE',  ( 30.44283453230164227, -2.188368138933637574, -4.533357778048659803 ) ) ;
#9916 = CARTESIAN_POINT ( 'NONE',  ( 33.09223089549517738, -4.049888575955752579, -8.283357778048662468 ) ) ;
#9917 = DIRECTION ( 'NONE',  ( 0.000000000000000000, 0.000000000000000000, -1.000000000000000000 ) ) ;
#9918 = CARTESIAN_POINT ( 'NONE',  ( -31.74999999999995737, 0.000000000000000000, 2.500000000000000444 ) ) ;
#9919 = CARTESIAN_POINT ( 'NONE',  ( 29.78250536075762867, -6.329556739422670830, 4.705209693361159573 ) ) ;
#9920 = ADVANCED_FACE ( 'NONE', ( #7576, #2233 ), #14379, .T. ) ;
#9921 = ORIENTED_EDGE ( 'NONE', *, *, #2539, .T. ) ;
#9922 = ORIENTED_EDGE ( 'NONE', *, *, #16533, .T. ) ;
#9923 = CARTESIAN_POINT ( 'NONE',  ( 26.99805802979993885, -6.665027654307603022, 6.861505862736158257 ) ) ;
#9924 = FACE_OUTER_BOUND ( 'NONE', #15881, .T. ) ;
#9925 = DIRECTION ( 'NONE',  ( 0.000000000000000000, 0.000000000000000000, -1.000000000000000000 ) ) ;
#9926 = EDGE_CURVE ( 'NONE', #2813, #2213, #6207, .T. ) ;
#9927 = ORIENTED_EDGE ( 'NONE', *, *, #5868, .F. ) ;
#9928 = CARTESIAN_POINT ( 'NONE',  ( 27.78610916120306129, -6.570083055755264745, 6.861505862736157368 ) ) ;
#9929 = FACE_OUTER_BOUND ( 'NONE', #17380, .T. ) ;
#9930 = FACE_OUTER_BOUND ( 'NONE', #16421, .T. ) ;
#9931 = CARTESIAN_POINT ( 'NONE',  ( 0.000000000000000000, 0.000000000000000000, 12.00000000000000000 ) ) ;
#9932 = DIRECTION ( 'NONE',  ( -0.1196152422706618645, 0.9928203230275510771, 0.000000000000000000 ) ) ;
#9933 = CARTESIAN_POINT ( 'NONE',  ( 33.73390066541284682, -2.518766455766908940, -3.283357778048662023 ) ) ;
#9934 = CARTESIAN_POINT ( 'NONE',  ( 32.97402322492378346, -4.064130265842336165, -3.627061608673664672 ) ) ;
#9935 = CARTESIAN_POINT ( 'NONE',  ( 0.000000000000000000, 0.000000000000000000, -1.901951201008075243 ) ) ;
#9936 = DIRECTION ( 'NONE',  ( -0.9928203230275510771, -0.1196152422706609902, -9.614813431917821547E-17 ) ) ;
#9937 = FILL_AREA_STYLE_COLOUR ( '', #3803 ) ;
#9938 = CARTESIAN_POINT ( 'NONE',  ( 32.79901970863393501, -6.593096864778464017, -5.783357778048668685 ) ) ;
#9939 = VERTEX_POINT ( 'NONE', #4834 ) ;
#9940 = CARTESIAN_POINT ( 'NONE',  ( 26.62577407660990758, -3.575027854551694695, -3.627061608673662008 ) ) ;
#9941 = CARTESIAN_POINT ( 'NONE',  ( 29.82675284572052732, -1.925235199084722959, -5.113484796970855228 ) ) ;
#9942 = EDGE_CURVE ( 'NONE', #15303, #15953, #1766, .T. ) ;
#9943 = ORIENTED_EDGE ( 'NONE', *, *, #408, .T. ) ;
#9944 = ORIENTED_EDGE ( 'NONE', *, *, #12597, .T. ) ;
#9945 = CARTESIAN_POINT ( 'NONE',  ( 26.84461768998868436, -2.294720455324902542, 5.783357778048668685 ) ) ;
#9946 = EDGE_CURVE ( 'NONE', #12386, #1259, #7846, .T. ) ;
#9947 = ORIENTED_EDGE ( 'NONE', *, *, #5156, .T. ) ;
#9948 = CARTESIAN_POINT ( 'NONE',  ( 26.46816385032927599, -3.594016774262162262, -3.627061608673662896 ) ) ;
#9949 = CARTESIAN_POINT ( 'NONE',  ( 45.00000000000000711, -16.03270077640482683, 5.537981825772250843 ) ) ;
#9950 = DIRECTION ( 'NONE',  ( -0.000000000000000000, -0.000000000000000000, 1.000000000000000000 ) ) ;
#9951 = CARTESIAN_POINT ( 'NONE',  ( 33.69269431359690969, -6.158264969628857166, -4.533357778048668685 ) ) ;
#9952 = CARTESIAN_POINT ( 'NONE',  ( 31.45915434921569798, -2.992700983430681028, -7.939653947423660263 ) ) ;
#9953 = CARTESIAN_POINT ( 'NONE',  ( -2.345747346278106438, 3.264484291692491436, -0.01223254789873562572 ) ) ;
#9954 = CARTESIAN_POINT ( 'NONE',  ( -45.00000000000000711, 0.000000000000000000, 5.537981825772250843 ) ) ;
#9955 = DIRECTION ( 'NONE',  ( 0.6287809056569713118, 0.6925565483635240938, 0.3535533905932746745 ) ) ;
#9956 = ADVANCED_FACE ( 'NONE', ( #953 ), #7481, .T. ) ;
#9957 = LINE ( 'NONE', #15594, #13703 ) ;
#9958 = ORIENTED_EDGE ( 'NONE', *, *, #3636, .F. ) ;
#9959 = CARTESIAN_POINT ( 'NONE',  ( 30.13703915187255689, -4.405930820630744371, -7.939653947423662039 ) ) ;
#9960 = DIRECTION ( 'NONE',  ( -0.8660254037844363761, 0.5000000000000038858, 0.000000000000000000 ) ) ;
#9961 = CARTESIAN_POINT ( 'NONE',  ( -35.41536221060850664, -16.03270077640482683, -0.5379818257722508434 ) ) ;
#9962 = CARTESIAN_POINT ( 'NONE',  ( 35.41536221060850664, -16.03270077640482683, -0.5379818257722508434 ) ) ;
#9963 = CARTESIAN_POINT ( 'NONE',  ( 28.74176732417158320, -7.092112515190875044, 5.783357778048669573 ) ) ;
#9964 = EDGE_CURVE ( 'NONE', #2784, #17331, #17359, .T. ) ;
#9965 = CARTESIAN_POINT ( 'NONE',  ( 28.12379965168153362, -6.829206799398704675, 4.533357778048659803 ) ) ;
#9966 = DIRECTION ( 'NONE',  ( -0.1196152422706610735, 0.9928203230275511881, 0.000000000000000000 ) ) ;
#9967 = VERTEX_POINT ( 'NONE', #7840 ) ;
#9968 = CARTESIAN_POINT ( 'NONE',  ( 26.55511561737958814, -2.656761491791831187, 4.533357778048667797 ) ) ;
#9969 = CARTESIAN_POINT ( 'NONE',  ( 27.55969062878875064, -7.234529412811931515, -5.783357778048668685 ) ) ;
#9970 = ORIENTED_EDGE ( 'NONE', *, *, #4828, .T. ) ;
#9971 = CARTESIAN_POINT ( 'NONE',  ( -20.27735869291019810, -10.58859781672278899, -15.46157951461808189 ) ) ;
#9972 = ORIENTED_EDGE ( 'NONE', *, *, #17857, .F. ) ;
#9973 = CARTESIAN_POINT ( 'NONE',  ( 27.75966235412334981, -2.811446176820259879, -4.705209693361160461 ) ) ;
#9974 = EDGE_CURVE ( 'NONE', #3987, #13923, #590, .T. ) ;
#9975 = VERTEX_POINT ( 'NONE', #12081 ) ;
#9976 = ORIENTED_EDGE ( 'NONE', *, *, #17477, .T. ) ;
#9977 = ORIENTED_EDGE ( 'NONE', *, *, #16698, .F. ) ;
#9978 = CARTESIAN_POINT ( 'NONE',  ( 29.19137779418881351, -4.519864338893556877, -3.627061608673664672 ) ) ;
#9979 = FACE_OUTER_BOUND ( 'NONE', #868, .T. ) ;
#9980 = CARTESIAN_POINT ( 'NONE',  ( 39.99999999999999289, 0.000000000000000000, 0.000000000000000000 ) ) ;
#9981 = CARTESIAN_POINT ( 'NONE',  ( 8.776279441628796363, -6.799038105676699750, -2.000000000000000000 ) ) ;
#9982 = CARTESIAN_POINT ( 'NONE',  ( 31.24221605398236790, -5.726592414339752857, -8.283357778048662468 ) ) ;
#9983 = EDGE_CURVE ( 'NONE', #11718, #15344, #5220, .T. ) ;
#9984 = CARTESIAN_POINT ( 'NONE',  ( 26.01652455409633902, -4.902371455920926380, -5.783357778048663356 ) ) ;
#9985 = EDGE_CURVE ( 'NONE', #5245, #2179, #891, .T. ) ;
#9986 = ORIENTED_EDGE ( 'NONE', *, *, #12922, .T. ) ;
#9987 = CARTESIAN_POINT ( 'NONE',  ( 32.12473870642251939, -5.420393343910986594, 3.627061608673662896 ) ) ;
#9988 = CARTESIAN_POINT ( 'NONE',  ( 27.02867472334902033, -6.034368414549446058, 7.939653947423658487 ) ) ;
#9989 = PRESENTATION_STYLE_ASSIGNMENT (( #5642 ) ) ;
#9990 = CARTESIAN_POINT ( 'NONE',  ( 29.54600080245929306, -4.477139269648729325, 8.283357778048662468 ) ) ;
#9991 = ORIENTED_EDGE ( 'NONE', *, *, #6618, .F. ) ;
#9992 = CARTESIAN_POINT ( 'NONE',  ( 28.50956232500783472, -2.083930644370540985, 5.113484796970861446 ) ) ;
#9993 = DIRECTION ( 'NONE',  ( -1.000000000000000000, 0.000000000000000000, 0.000000000000000000 ) ) ;
#9994 = EDGE_CURVE ( 'NONE', #12240, #4518, #17428, .T. ) ;
#9995 = EDGE_LOOP ( 'NONE', ( #2695, #6907, #14856, #7398 ) ) ;
#9996 = CARTESIAN_POINT ( 'NONE',  ( 30.60493568430522160, -6.867637522466304212, -5.113484796970860558 ) ) ;
#9997 = EDGE_CURVE ( 'NONE', #16703, #364, #17128, .T. ) ;
#9998 = CARTESIAN_POINT ( 'NONE',  ( 26.63030083514515312, -6.709335133632020387, -6.861505862736167138 ) ) ;
#9999 = CARTESIAN_POINT ( 'NONE',  ( 30.66050125466253107, -2.889050389913576655, -3.283357778048662023 ) ) ;
#10000 = DIRECTION ( 'NONE',  ( -0.1196152422706606572, 0.9928203230275512992, 0.000000000000000000 ) ) ;
#10001 = ITEM_DEFINED_TRANSFORMATION ( 'NONE', 'NONE', #1031,  #3575 ) ;
#10002 = DIRECTION ( 'NONE',  ( 0.000000000000000000, 0.000000000000000000, -1.000000000000000000 ) ) ;
#10003 = CARTESIAN_POINT ( 'NONE',  ( 28.28502977505876359, -2.748149777785362957, -6.861505862736158257 ) ) ;
#10004 = CARTESIAN_POINT ( 'NONE',  ( 32.28234893270314387, -5.401404424200516807, -7.939653947423664704 ) ) ;
#10005 = CYLINDRICAL_SURFACE ( 'NONE', #9605, 2.499999999999999112 ) ;
#10006 = DIRECTION ( 'NONE',  ( 0.000000000000000000, 0.000000000000000000, 1.000000000000000000 ) ) ;
#10007 = CARTESIAN_POINT ( 'NONE',  ( 30.28142597461332741, -2.507623461452779701, 6.861505862736166250 ) ) ;
#10008 = ORIENTED_EDGE ( 'NONE', *, *, #6072, .F. ) ;
#10009 = EDGE_LOOP ( 'NONE', ( #5412, #11608, #812, #13666 ) ) ;
#10010 = CARTESIAN_POINT ( 'NONE',  ( 27.30005507882132676, -4.747731375419166788, -3.627061608673664672 ) ) ;
#10011 = ORIENTED_EDGE ( 'NONE', *, *, #12558, .T. ) ;
#10012 = CARTESIAN_POINT ( 'NONE',  ( 28.86293393808771057, -2.678523738846987357, 6.861505862736165362 ) ) ;
#10013 = CARTESIAN_POINT ( 'NONE',  ( 31.08763465596552322, -1.773323841400983758, -5.113484796970854340 ) ) ;
#10014 = CYLINDRICAL_SURFACE ( 'NONE', #17502, 2.749999999999992895 ) ;
#10015 = EDGE_LOOP ( 'NONE', ( #12656, #10397, #3442, #6567, #2551, #9922, #6925 ) ) ;
#10016 = SURFACE_STYLE_USAGE ( .BOTH. , #11375 ) ;
#10017 = CARTESIAN_POINT ( 'NONE',  ( -4.000000000000000000, 1.677751148815738391, -3.235249634003040775 ) ) ;
#10018 = CARTESIAN_POINT ( 'NONE',  ( 2.500000000000000000, 2.357898499370432166, -2.385244779468109755E-15 ) ) ;
#10019 = CARTESIAN_POINT ( 'NONE',  ( 8.409399735147211686E-16, 4.618802153517009401, -3.133295621305383083 ) ) ;
#10020 =( REPRESENTATION_RELATIONSHIP ('NONE','NONE', #3227, #16332 ) REPRESENTATION_RELATIONSHIP_WITH_TRANSFORMATION ( #3668 )SHAPE_REPRESENTATION_RELATIONSHIP( ) );
#10021 = DIRECTION ( 'NONE',  ( 0.000000000000000000, 0.000000000000000000, 1.000000000000000000 ) ) ;
#10023 = ADVANCED_FACE ( 'NONE', ( #3007, #4797 ), #8714, .T. ) ;
#10022 = CARTESIAN_POINT ( 'NONE',  ( 26.83664947211162399, -6.984282976826746037, -4.533357778048668685 ) ) ;
#10024 = CARTESIAN_POINT ( 'NONE',  ( -3.347071143357316814, -15.22052928361022950, 17.00000000000000000 ) ) ;
#10025 = DIRECTION ( 'NONE',  ( -1.000000000000000000, -0.000000000000000000, -0.000000000000000000 ) ) ;
#10026 = PRESENTATION_STYLE_ASSIGNMENT (( #14039 ) ) ;
#10027 = CARTESIAN_POINT ( 'NONE',  ( 32.01513846370018967, -2.298745344637636912, -4.705209693361161349 ) ) ;
#10028 = EDGE_CURVE ( 'NONE', #14403, #13578, #10803, .T. ) ;
#10029 = CARTESIAN_POINT ( 'NONE',  ( 26.10492286888475633, -5.636087676172646610, -8.120510362352304057 ) ) ;
#10030 = CYLINDRICAL_SURFACE ( 'NONE', #17962, 2.000000000000001776 ) ;
#10031 = EDGE_LOOP ( 'NONE', ( #4127, #13040, #10536, #14059 ) ) ;
#10032 = VERTEX_POINT ( 'NONE', #10319 ) ;
#10033 = ORIENTED_EDGE ( 'NONE', *, *, #2887, .F. ) ;
#10034 = VERTEX_POINT ( 'NONE', #467 ) ;
#10035 = CARTESIAN_POINT ( 'NONE',  ( 29.50659824675005893, -4.481886499472614638, 3.627061608673664228 ) ) ;
#10036 = CARTESIAN_POINT ( 'NONE',  ( 31.21213704492286212, -2.822589171134389563, 8.283357778048666020 ) ) ;
#10037 = CARTESIAN_POINT ( 'NONE',  ( 26.31176419598820360, -7.352894575460818594, 5.384699358761103838 ) ) ;
#10038 = VECTOR ( 'NONE', #4735, 1000.000000000000000 ) ;
#10039 = CARTESIAN_POINT ( 'NONE',  ( 15.92260893619738837, -28.39189527176317540, 12.00000000000000000 ) ) ;
#10040 = LINE ( 'NONE', #8605, #3821 ) ;
#10041 = CARTESIAN_POINT ( 'NONE',  ( 33.46007730730551799, -5.886481946178435010, -4.705209693361169343 ) ) ;
#10042 = CARTESIAN_POINT ( 'NONE',  ( 29.16815758536418102, -2.004582921727632971, -5.783357778048664244 ) ) ;
#10043 = DIRECTION ( 'NONE',  ( 1.000000000000000000, 0.000000000000000000, 0.000000000000000000 ) ) ;
#10044 = EDGE_CURVE ( 'NONE', #2932, #15540, #17068, .T. ) ;
#10045 = CARTESIAN_POINT ( 'NONE',  ( 20.25000000000001066, -16.21813761408365195, -13.00000000000000355 ) ) ;
#10046 = CARTESIAN_POINT ( 'NONE',  ( -11.16099250167134826, 15.37423824781781079, 16.67067991271537863 ) ) ;
#10047 = VERTEX_POINT ( 'NONE', #10144 ) ;
#10048 = CARTESIAN_POINT ( 'NONE',  ( 30.88125018618674744, -3.062327022369072171, -3.627061608673662896 ) ) ;
#10049 = DIRECTION ( 'NONE',  ( 0.000000000000000000, 0.000000000000000000, 1.000000000000000000 ) ) ;
#10050 = CARTESIAN_POINT ( 'NONE',  ( 32.26971135134834867, -1.630906943779925955, -5.113484796970855228 ) ) ;
#10051 = CYLINDRICAL_SURFACE ( 'NONE', #7772, 6.249999999999998224 ) ;
#10052 = ORIENTED_EDGE ( 'NONE', *, *, #6195, .T. ) ;
#10053 = ADVANCED_FACE ( 'NONE', ( #5973 ), #11597, .F. ) ;
#10054 = CARTESIAN_POINT ( 'NONE',  ( 25.96530230012339757, -2.390463732198628399, 6.453230759126474148 ) ) ;
#10055 = CARTESIAN_POINT ( 'NONE',  ( 27.15176839919044482, -1.857969822100365098, 5.783357778048668685 ) ) ;
#10056 = CARTESIAN_POINT ( 'NONE',  ( 25.95642634701329499, -4.403549397486667516, -3.686412874245489135 ) ) ;
#10057 = ORIENTED_EDGE ( 'NONE', *, *, #10749, .F. ) ;
#10058 = DIRECTION ( 'NONE',  ( -0.1196152422706610735, 0.9928203230275511881, 0.000000000000000000 ) ) ;
#10059 = ORIENTED_EDGE ( 'NONE', *, *, #16598, .T. ) ;
#10060 = ORIENTED_EDGE ( 'NONE', *, *, #10958, .F. ) ;
#10061 = LINE ( 'NONE', #16620, #31 ) ;
#10062 = ORIENTED_EDGE ( 'NONE', *, *, #14569, .F. ) ;
#10063 = PRESENTATION_LAYER_ASSIGNMENT (  '', '', ( #17928 ) ) ;
#10064 = CARTESIAN_POINT ( 'NONE',  ( 0.000000000000000000, 0.000000000000000000, -1.901951201008075243 ) ) ;
#10065 = VECTOR ( 'NONE', #334, 1000.000000000000227 ) ;
#10066 = VERTEX_POINT ( 'NONE', #7181 ) ;
#10067 = ORIENTED_EDGE ( 'NONE', *, *, #592, .F. ) ;
#10068 = CARTESIAN_POINT ( 'NONE',  ( 31.27962407439061110, -2.387360303286481855, -6.861505862736159145 ) ) ;
#10069 = DIRECTION ( 'NONE',  ( -0.000000000000000000, 1.000000000000000000, -0.000000000000000000 ) ) ;
#10070 = CARTESIAN_POINT ( 'NONE',  ( 29.27960797773944179, -6.689954721521948144, -4.533357778048668685 ) ) ;
#10071 = DIRECTION ( 'NONE',  ( -1.000000000000000000, 0.000000000000000000, 0.000000000000000000 ) ) ;
#10072 = VERTEX_POINT ( 'NONE', #4712 ) ;
#10073 = VECTOR ( 'NONE', #6993, 999.9999999999998863 ) ;
#10074 = CARTESIAN_POINT ( 'NONE',  ( 32.26287188679368967, -2.695996373064596607, -8.283357778048658915 ) ) ;
#10075 = DIRECTION ( 'NONE',  ( 1.000000000000000000, 0.000000000000000000, 0.000000000000000000 ) ) ;
#10076 = ORIENTED_EDGE ( 'NONE', *, *, #10556, .T. ) ;
#10077 = CARTESIAN_POINT ( 'NONE',  ( 26.03726795043090547, -3.446058701420613879, 3.283357778048666464 ) ) ;
#10078 = VECTOR ( 'NONE', #13932, 1000.000000000000000 ) ;
#10079 = ADVANCED_FACE ( 'NONE', ( #10240 ), #11311, .T. ) ;
#10080 = CARTESIAN_POINT ( 'NONE',  ( -24.62400252878131113, -22.25686381702613659, 14.56428162264008286 ) ) ;
#10081 = CARTESIAN_POINT ( 'NONE',  ( 32.92264866086529906, -1.552240892477451784, 5.113484796970859669 ) ) ;
#10082 = ORIENTED_EDGE ( 'NONE', *, *, #9707, .F. ) ;
#10083 = ORIENTED_EDGE ( 'NONE', *, *, #14298, .T. ) ;
#10084 = LINE ( 'NONE', #15636, #8098 ) ;
#10085 = EDGE_CURVE ( 'NONE', #7303, #11429, #11594, .T. ) ;
#10086 = CARTESIAN_POINT ( 'NONE',  ( 26.30108762358334928, -7.264277791658039440, -6.611981523323152032 ) ) ;
#10087 = EDGE_LOOP ( 'NONE', ( #16850, #3860, #17086, #11688, #14910 ) ) ;
#10088 = ORIENTED_EDGE ( 'NONE', *, *, #8326, .F. ) ;
#10089 = DIRECTION ( 'NONE',  ( -1.000000000000000000, 0.000000000000000000, 0.000000000000000000 ) ) ;
#10090 = VECTOR ( 'NONE', #17136, 1000.000000000000000 ) ;
#10091 = CARTESIAN_POINT ( 'NONE',  ( 32.93832978346670615, -1.887710243310447567, -7.033357778048658027 ) ) ;
#10092 = CARTESIAN_POINT ( 'NONE',  ( -4.000000000000000000, 0.3987449864459981508, -0.01220643443059921812 ) ) ;
#10093 = SHAPE_DEFINITION_REPRESENTATION ( #17552, #2651 ) ;
#10094 = CARTESIAN_POINT ( 'NONE',  ( 0.000000000000000000, 0.000000000000000000, -2.000000000000000000 ) ) ;
#10095 = CARTESIAN_POINT ( 'NONE',  ( 29.13014440709066832, -5.781182818409868140, -7.939653947423664704 ) ) ;
#10096 = CARTESIAN_POINT ( 'NONE',  ( 32.82963640218302004, -5.962437625020304388, -4.705209693361169343 ) ) ;
#10097 = DIRECTION ( 'NONE',  ( -0.1196152422706611984, 0.9928203230275510771, 0.000000000000000000 ) ) ;
#10098 = CARTESIAN_POINT ( 'NONE',  ( 0.000000000000000000, 0.000000000000000000, -10.00000000000000000 ) ) ;
#10099 = CARTESIAN_POINT ( 'NONE',  ( 28.71854711534694715, -4.576831098024959132, 7.939653947423662039 ) ) ;
#10100 = ADVANCED_FACE ( 'NONE', ( #8809 ), #15786, .T. ) ;
#10101 = VERTEX_POINT ( 'NONE', #16888 ) ;
#10102 = AXIS2_PLACEMENT_3D ( 'NONE', #5315, #2521, #1528 ) ;
#10103 = CARTESIAN_POINT ( 'NONE',  ( 26.24062359194589078, -6.129313013101781671, -3.627061608673667781 ) ) ;
#10104 = ORIENTED_EDGE ( 'NONE', *, *, #4806, .F. ) ;
#10105 = CARTESIAN_POINT ( 'NONE',  ( 31.55553118839817728, -4.235030543236534939, 3.627061608673664228 ) ) ;
#10106 = CARTESIAN_POINT ( 'NONE',  ( 25.71748644841968456, -2.420320648352046078, 5.783357778048663356 ) ) ;
#10107 = CARTESIAN_POINT ( 'NONE',  ( -45.50000000000000000, -19.03270077640483038, -5.537981825772250843 ) ) ;
#10108 = ORIENTED_EDGE ( 'NONE', *, *, #4941, .F. ) ;
#10109 = CARTESIAN_POINT ( 'NONE',  ( 32.83754810739939956, -9.116730809865838836, -5.783357778048662468 ) ) ;
#10110 = CARTESIAN_POINT ( 'NONE',  ( 35.74085044863416982, -18.73429073671341172, 11.27079897466147251 ) ) ;
#10111 = FACE_OUTER_BOUND ( 'NONE', #7325, .T. ) ;
#10112 = AXIS2_PLACEMENT_3D ( 'NONE', #12642, #328, #232 ) ;
#10113 = CIRCLE ( 'NONE', #17690, 5.000000000000000000 ) ;
#10114 = CARTESIAN_POINT ( 'NONE',  ( -25.07353123778395343, 1.235291682954730463, -14.60266621045499669 ) ) ;
#10115 = CARTESIAN_POINT ( 'NONE',  ( 26.10855331130634127, -2.710563430764044490, -4.533357778048659803 ) ) ;
#10116 = CARTESIAN_POINT ( 'NONE',  ( 28.77507474356526984, -18.63405514100518801, 13.50648245236009792 ) ) ;
#10117 = DIRECTION ( 'NONE',  ( 0.000000000000000000, -1.000000000000000000, 0.000000000000000000 ) ) ;
#10118 = CARTESIAN_POINT ( 'NONE',  ( 31.25770402584614516, -1.763030703431812674, -5.783357778048658027 ) ) ;
#10119 = ORIENTED_EDGE ( 'NONE', *, *, #2231, .F. ) ;
#10120 = AXIS2_PLACEMENT_3D ( 'NONE', #7304, #4563, #9907 ) ;
#10121 = CARTESIAN_POINT ( 'NONE',  ( 25.84832697747033592, -3.506312147857040706, -7.581167935121603918 ) ) ;
#10122 = CARTESIAN_POINT ( 'NONE',  ( 29.78612525785423060, -2.267488637519798012, 4.533357778048667797 ) ) ;
#10123 = EDGE_CURVE ( 'NONE', #5056, #5499, #283, .T. ) ;
#10124 = ORIENTED_EDGE ( 'NONE', *, *, #1378, .F. ) ;
#10125 = EDGE_LOOP ( 'NONE', ( #10126, #14543, #16749, #12783 ) ) ;
#10126 = ORIENTED_EDGE ( 'NONE', *, *, #12099, .F. ) ;
#10127 =( BOUNDED_CURVE ( )  B_SPLINE_CURVE ( 2, ( #3512, #16128, #7865, #10642, #6414, #11931, #11665, #6503, #16043 ),
 .UNSPECIFIED., .F., .T. ) 
 B_SPLINE_CURVE_WITH_KNOTS ( ( 3, 2, 2, 2, 3 ),
 ( 0.6346153846153846922, 0.6410256410256410797, 0.6538461538461538547, 0.6666666666666666297, 0.6730769230769231282 ),
 .UNSPECIFIED. ) 
 CURVE ( )  GEOMETRIC_REPRESENTATION_ITEM ( )  RATIONAL_B_SPLINE_CURVE ( ( 0.9330127018922192983, 0.9330127018922198534, 1.000000000000000000, 0.8660254037844387076, 1.000000000000000000, 0.8660254037844387076, 1.000000000000000000, 0.9330127018922187432, 0.9330127018922192983 ) ) 
 REPRESENTATION_ITEM ( '' )  );
#10128 = ORIENTED_EDGE ( 'NONE', *, *, #15724, .T. ) ;
#10129 = CARTESIAN_POINT ( 'NONE',  ( 28.34209327568754944, -5.876127416962207306, 3.627061608673662896 ) ) ;
#10130 = CARTESIAN_POINT ( 'NONE',  ( -13.00000000000000178, -1.592040838891559293E-15, 8.700000000000001066 ) ) ;
#10131 = DIRECTION ( 'NONE',  ( 0.9928203230275512992, 0.1196152422706614898, -0.000000000000000000 ) ) ;
#10132 = CLOSED_SHELL ( 'NONE', ( #3095, #2358, #2758, #13772 ) ) ;
#10133 = FACE_OUTER_BOUND ( 'NONE', #4117, .T. ) ;
#10134 = STYLED_ITEM ( 'NONE', ( #14519 ), #7018 ) ;
#10135 = CARTESIAN_POINT ( 'NONE',  ( -21.03357387009699409, -22.15422581635157684, -15.32066355758547083 ) ) ;
#10136 = CARTESIAN_POINT ( 'NONE',  ( 32.32618902979206865, -6.650063623909865385, -5.783357778048669573 ) ) ;
#10137 = CARTESIAN_POINT ( 'NONE',  ( 31.71123609653335507, -2.762457591843783256, -8.283357778048660691 ) ) ;
#10138 = FACE_OUTER_BOUND ( 'NONE', #8768, .T. ) ;
#10139 = CARTESIAN_POINT ( 'NONE',  ( 0.000000000000000000, 0.000000000000000000, -6.000000000000000000 ) ) ;
#10140 = PLANE ( 'NONE',  #1227 ) ;
#10141 = CARTESIAN_POINT ( 'NONE',  ( -14.05523583925745257, 13.74128089903392613, 16.39434919531312218 ) ) ;
#10142 = CIRCLE ( 'NONE', #2912, 1.000000000000000000 ) ;
#10143 = CARTESIAN_POINT ( 'NONE',  ( 27.93049598394382116, -4.671775696577297410, -3.627061608673664672 ) ) ;
#10144 = CARTESIAN_POINT ( 'NONE',  ( -29.25000000000000000, -16.21813761408365195, 13.37255996287876947 ) ) ;
#10145 = PLANE ( 'NONE',  #11790 ) ;
#10146 = CARTESIAN_POINT ( 'NONE',  ( 26.11428532722776197, -5.713797161519015511, -3.668609639089262409 ) ) ;
#10147 = DIRECTION ( 'NONE',  ( 1.000000000000000000, 0.000000000000000000, 0.000000000000000000 ) ) ;
#10148 = VECTOR ( 'NONE', #11683, 1000.000000000000000 ) ;
#10149 = PRESENTATION_LAYER_ASSIGNMENT (  '', '', ( #7852 ) ) ;
#10150 = CARTESIAN_POINT ( 'NONE',  ( 28.28511899221430070, -4.629050627332469858, 8.283357778048662468 ) ) ;
#10151 = CARTESIAN_POINT ( 'NONE',  ( 26.49461065740898391, -7.352653653197164907, -5.783357778048668685 ) ) ;
#10152 = EDGE_CURVE ( 'NONE', #5499, #10872, #3792, .T. ) ;
#10153 = EDGE_LOOP ( 'NONE', ( #6116, #11029, #14894, #2516 ) ) ;
#10154 = AXIS2_PLACEMENT_3D ( 'NONE', #4171, #8323, #9500 ) ;
#10155 = DIRECTION ( 'NONE',  ( 0.000000000000000000, 1.000000000000000000, 3.469446951953614189E-16 ) ) ;
#10156 = EDGE_LOOP ( 'NONE', ( #6325, #4298, #6059, #6544 ) ) ;
#10157 = CARTESIAN_POINT ( 'NONE',  ( 33.15485366002904755, -6.560422763297783177, -5.783357778048663356 ) ) ;
#10158 = EDGE_CURVE ( 'NONE', #8959, #729, #7366, .T. ) ;
#10159 = ORIENTED_EDGE ( 'NONE', *, *, #8777, .F. ) ;
#10160 = ADVANCED_FACE ( 'NONE', ( #3362 ), #15510, .F. ) ;
#10161 = AXIS2_PLACEMENT_3D ( 'NONE', #15231, #6620, #10858 ) ;
#10162 = CARTESIAN_POINT ( 'NONE',  ( 27.02867472334902033, -6.034368414549445170, -3.627061608673668225 ) ) ;
#10163 = CARTESIAN_POINT ( 'NONE',  ( 26.62577407660990758, -3.575027854551694695, -3.627061608673662008 ) ) ;
#10164 = ORIENTED_EDGE ( 'NONE', *, *, #15211, .F. ) ;
#10165 = CARTESIAN_POINT ( 'NONE',  ( 28.56093688906631911, -4.595820017735426255, -3.627061608673664672 ) ) ;
#10166 = AXIS2_PLACEMENT_3D ( 'NONE', #12414, #12509, #8331 ) ;
#10167 = DIRECTION ( 'NONE',  ( -0.1196152422706626278, 0.9928203230275510771, 0.000000000000000000 ) ) ;
#10168 = CARTESIAN_POINT ( 'NONE',  ( 29.34405387406022570, -7.019548880150045633, -5.113484796970862334 ) ) ;
#10169 = CARTESIAN_POINT ( 'NONE',  ( 36.27615609941022257, -23.17738945083361557, 12.00000000000000000 ) ) ;
#10170 = CIRCLE ( 'NONE', #6997, 5.500000000000000888 ) ;
#10171 = ORIENTED_EDGE ( 'NONE', *, *, #13028, .T. ) ;
#10172 = CARTESIAN_POINT ( 'NONE',  ( 30.58169613980036772, -2.898544849976259385, -3.283357778048662023 ) ) ;
#10173 = PLANE ( 'NONE',  #2257 ) ;
#10174 = CARTESIAN_POINT ( 'NONE',  ( 32.79901970863393501, -6.593096864778464017, 5.783357778048658027 ) ) ;
#10175 = CIRCLE ( 'NONE', #5252, 10.50000000000000000 ) ;
#10176 = ADVANCED_FACE ( 'NONE', ( #3092 ), #17261, .F. ) ;
#10177 = CARTESIAN_POINT ( 'NONE',  ( 5.781152949374519956, -1.605699403978931850, -3.000000000000000888 ) ) ;
#10178 = DIRECTION ( 'NONE',  ( -0.000000000000000000, -0.000000000000000000, -1.000000000000000000 ) ) ;
#10179 = CARTESIAN_POINT ( 'NONE',  ( 29.08935247050201767, -2.014077381790315702, 5.783357778048667797 ) ) ;
#10180 = EDGE_CURVE ( 'NONE', #7075, #3342, #1457, .T. ) ;
#10181 = EDGE_LOOP ( 'NONE', ( #11392, #5979, #3930, #14896 ) ) ;
#10182 = CARTESIAN_POINT ( 'NONE',  ( 25.41044654184514329, -5.982623484807521486, -5.783357778048664244 ) ) ;
#10183 = ORIENTED_EDGE ( 'NONE', *, *, #15758, .T. ) ;
#10184 = CARTESIAN_POINT ( 'NONE',  ( 7.374038404635976818, 5.989453865500072638, -2.000000000000000000 ) ) ;
#10185 = CARTESIAN_POINT ( 'NONE',  ( 26.64639396487419987, -2.308405637095112706, -5.783357778048658027 ) ) ;
#10186 = VECTOR ( 'NONE', #16392, 1000.000000000000000 ) ;
#10187 = CIRCLE ( 'NONE', #13683, 13.00000000000000178 ) ;
#10188 = EDGE_CURVE ( 'NONE', #3946, #3342, #7382, .T. ) ;
#10189 = CARTESIAN_POINT ( 'NONE',  ( 32.51061761821408425, -6.300681867249914525, -4.533357778048668685 ) ) ;
#10190 = DIRECTION ( 'NONE',  ( -1.000000000000000000, 0.000000000000000000, 0.000000000000000000 ) ) ;
#10191 = SHAPE_DEFINITION_REPRESENTATION ( #9529, #2081 ) ;
#10192 = CARTESIAN_POINT ( 'NONE',  ( 8.472608240843633681E-22, -7.722472891792491889E-22, -7.794427190999915211 ) ) ;
#10193 = CARTESIAN_POINT ( 'NONE',  ( 32.80318959510331212, -2.203800746085299522, -4.705209693361160461 ) ) ;
#10194 = CARTESIAN_POINT ( 'NONE',  ( 27.22618411036838637, -2.238552374514887866, -5.113484796970851676 ) ) ;
#10195 = FACE_OUTER_BOUND ( 'NONE', #14851, .T. ) ;
#10196 = VECTOR ( 'NONE', #10744, 1000.000000000000114 ) ;
#10197 = CARTESIAN_POINT ( 'NONE',  ( 29.14753769709988518, -3.271205139184214516, 7.939653947423664704 ) ) ;
#10198 = ADVANCED_FACE ( 'NONE', ( #11573, #2986 ), #5774, .T. ) ;
#10199 = AXIS2_PLACEMENT_3D ( 'NONE', #11808, #15537, #14180 ) ;
#10200 = ORIENTED_EDGE ( 'NONE', *, *, #10647, .F. ) ;
#10201 = CONICAL_SURFACE ( 'NONE', #7622, 3.999999999999986677, 0.7853981633974400633 ) ;
#10202 = CARTESIAN_POINT ( 'NONE',  ( 25.83772294520678159, -3.669972453104032084, -3.627061608673662896 ) ) ;
#10203 = EDGE_LOOP ( 'NONE', ( #2158, #13496, #16171, #395, #14568 ) ) ;
#10204 = CARTESIAN_POINT ( 'NONE',  ( 26.35439372113758694, -4.861664893681965083, 3.627061608673664228 ) ) ;
#10205 = CARTESIAN_POINT ( 'NONE',  ( 31.97277696464621854, -6.702839660918840536, -5.783357778048663356 ) ) ;
#10206 = DIRECTION ( 'NONE',  ( -0.06446199418653550395, -0.9979201627913403261, -4.248110196704583871E-22 ) ) ;
#10207 = ORIENTED_EDGE ( 'NONE', *, *, #17843, .T. ) ;
#10208 = CARTESIAN_POINT ( 'NONE',  ( 32.83754810739938534, -9.116730809865837060, 4.216642221951339309 ) ) ;
#10209 = CYLINDRICAL_SURFACE ( 'NONE', #11572, 2.500000000000001776 ) ;
#10210 = CYLINDRICAL_SURFACE ( 'NONE', #12212, 25.00000000000000000 ) ;
#10211 = CARTESIAN_POINT ( 'NONE',  ( 32.26287188679368256, -2.695996373064596607, -8.283357778048660691 ) ) ;
#10212 = CARTESIAN_POINT ( 'NONE',  ( 27.53837573810956130, -6.172832027328289506, -8.283357778048662468 ) ) ;
#10213 = EDGE_CURVE ( 'NONE', #3807, #3702, #11395, .T. ) ;
#10214 = FACE_OUTER_BOUND ( 'NONE', #9652, .T. ) ;
#10215 = CARTESIAN_POINT ( 'NONE',  ( 0.000000000000000000, 0.000000000000000000, -3.000000000000002665 ) ) ;
#10216 = CARTESIAN_POINT ( 'NONE',  ( 29.60297508593253468, -5.724216059278466773, -7.939653947423664704 ) ) ;
#10217 = CARTESIAN_POINT ( 'NONE',  ( 26.60838078660069428, -6.085005533777348319, -7.939653947423662927 ) ) ;
#10218 = CARTESIAN_POINT ( 'NONE',  ( 32.58190297908952004, -5.565186596593329149, 3.283357778048663800 ) ) ;
#10219 = ADVANCED_FACE ( 'NONE', ( #14126 ), #358, .T. ) ;
#10220 = CIRCLE ( 'NONE', #8201, 13.00000000000000178 ) ;
#10221 = EDGE_CURVE ( 'NONE', #3677, #1847, #12673, .T. ) ;
#10222 = ORIENTED_EDGE ( 'NONE', *, *, #9478, .T. ) ;
#10223 = VERTEX_POINT ( 'NONE', #4777 ) ;
#10224 = ORIENTED_EDGE ( 'NONE', *, *, #13003, .F. ) ;
#10225 = CARTESIAN_POINT ( 'NONE',  ( 33.14902674121363901, -1.535163666906202318, 5.783357778048668685 ) ) ;
#10226 = CARTESIAN_POINT ( 'NONE',  ( 32.29974222271236073, -2.891426744974864071, 7.939653947423662927 ) ) ;
#10227 = CARTESIAN_POINT ( 'NONE',  ( -20.00000000000000000, 7.999999999999996447, -15.51150668642334374 ) ) ;
#10228 = CARTESIAN_POINT ( 'NONE',  ( -28.68370877339674863, -18.82577899785919584, -13.53184763361698906 ) ) ;
#10229 = CARTESIAN_POINT ( 'NONE',  ( 26.49461065740898036, -7.352653653197164019, -5.783357778048668685 ) ) ;
#10230 = DIRECTION ( 'NONE',  ( 0.000000000000000000, 0.000000000000000000, -1.000000000000000000 ) ) ;
#10231 = CARTESIAN_POINT ( 'NONE',  ( 0.000000000000000000, 0.000000000000000000, -3.000000000000000000 ) ) ;
#10232 = DIRECTION ( 'NONE',  ( 0.000000000000000000, 0.000000000000000000, -1.000000000000000000 ) ) ;
#10233 = EDGE_CURVE ( 'NONE', #947, #6789, #10299, .T. ) ;
#10234 = CARTESIAN_POINT ( 'NONE',  ( 26.39379627684682106, -4.856917663858078882, -3.283357778048664688 ) ) ;
#10235 = EDGE_CURVE ( 'NONE', #14350, #12819, #20, .T. ) ;
#10236 = ORIENTED_EDGE ( 'NONE', *, *, #12774, .T. ) ;
#10237 = ORIENTED_EDGE ( 'NONE', *, *, #1673, .F. ) ;
#10238 = CARTESIAN_POINT ( 'NONE',  ( 25.71072941247523502, -3.058302133056337357, -4.705209693361161349 ) ) ;
#10239 = CIRCLE ( 'NONE', #12854, 10.50000000000000000 ) ;
#10240 = FACE_OUTER_BOUND ( 'NONE', #1288, .T. ) ;
#10241 = FACE_OUTER_BOUND ( 'NONE', #14505, .T. ) ;
#10242 = CARTESIAN_POINT ( 'NONE',  ( 27.33945763453056088, -4.742984145595265488, 3.283357778048664244 ) ) ;
#10243 = ORIENTED_EDGE ( 'NONE', *, *, #15614, .F. ) ;
#10244 = CARTESIAN_POINT ( 'NONE',  ( 23.02601376483258022, 3.965314980223224151, 6.000000000000000000 ) ) ;
#10245 = CARTESIAN_POINT ( 'NONE',  ( 31.51169109130924184, -2.986371343527201905, -3.627061608673662896 ) ) ;
#10246 = ORIENTED_EDGE ( 'NONE', *, *, #14726, .T. ) ;
#10247 = CARTESIAN_POINT ( 'NONE',  ( 29.45101334415624095, -7.006662376286321603, -5.783357778048657138 ) ) ;
#10248 = CARTESIAN_POINT ( 'NONE',  ( 25.79194807336802953, -3.038360733637177624, -6.974889548725401234 ) ) ;
#10249 = CARTESIAN_POINT ( 'NONE',  ( -34.91600907648203389, -11.88801210197604341, -11.56671555609732671 ) ) ;
#10250 = CARTESIAN_POINT ( 'NONE',  ( 27.63266882139180325, -2.199775856772564708, -5.783357778048658915 ) ) ;
#10251 = CARTESIAN_POINT ( 'NONE',  ( 27.28266178881210280, -7.257709054644824853, -5.783357778048669573 ) ) ;
#10252 = ADVANCED_FACE ( 'NONE', ( #6419 ), #8413, .T. ) ;
#10253 = CARTESIAN_POINT ( 'NONE',  ( 27.72904566057427189, -3.442105416578422172, -3.627061608673662896 ) ) ;
#10254 = CARTESIAN_POINT ( 'NONE',  ( -45.50000000000000000, -16.03270077640482683, 2.787981825772262390 ) ) ;
#10255 = CARTESIAN_POINT ( 'NONE',  ( 33.13353876934985465, -5.498725377814142057, -8.283357778048664244 ) ) ;
#10256 = FACE_OUTER_BOUND ( 'NONE', #17404, .T. ) ;
#10257 = CARTESIAN_POINT ( 'NONE',  ( 28.41265020943543362, -1.706058464416624787, -5.783357778048658027 ) ) ;
#10258 =( BOUNDED_CURVE ( )  B_SPLINE_CURVE ( 2, ( #15062, #13710, #16695, #4272, #6815, #2258, #4622, #12882, #14249 ),
 .UNSPECIFIED., .F., .T. ) 
 B_SPLINE_CURVE_WITH_KNOTS ( ( 3, 2, 2, 2, 3 ),
 ( 0.8653846153846154188, 0.8717948717948718063, 0.8846153846153845812, 0.8974358974358974672, 0.9038461538461538547 ),
 .UNSPECIFIED. ) 
 CURVE ( )  GEOMETRIC_REPRESENTATION_ITEM ( )  RATIONAL_B_SPLINE_CURVE ( ( 0.9330127018922192983, 0.9330127018922198534, 1.000000000000000000, 0.8660254037844387076, 1.000000000000000000, 0.8660254037844387076, 1.000000000000000000, 0.9330127018922194093, 0.9330127018922194093 ) ) 
 REPRESENTATION_ITEM ( '' )  );
#10259 = CARTESIAN_POINT ( 'NONE',  ( 31.89397184978405519, -6.712334120981523711, -5.783357778048663356 ) ) ;
#10260 = EDGE_CURVE ( 'NONE', #15308, #1274, #15117, .T. ) ;
#10261 = CARTESIAN_POINT ( 'NONE',  ( 26.24741491880507027, -3.420740141806666745, 8.283357778048664244 ) ) ;
#10262 = ORIENTED_EDGE ( 'NONE', *, *, #17889, .T. ) ;
#10263 = EDGE_LOOP ( 'NONE', ( #8622, #3925, #11762, #16443 ) ) ;
#10264 = CARTESIAN_POINT ( 'NONE',  ( -13.00000000000000178, -1.592040838891559293E-15, 12.00000000000000000 ) ) ;
#10265 = DIRECTION ( 'NONE',  ( 0.9928203230275514102, 0.1196152422706598939, 0.000000000000000000 ) ) ;
#10266 = CARTESIAN_POINT ( 'NONE',  ( 8.249999999999971578, -6.495190528383328221, -3.000000000000002665 ) ) ;
#10267 = VERTEX_POINT ( 'NONE', #983 ) ;
#10268 =( BOUNDED_CURVE ( )  B_SPLINE_CURVE ( 2, ( #9812, #5647, #4301, #14094, #15362, #2944, #8656, #7125, #226 ),
 .UNSPECIFIED., .F., .T. ) 
 B_SPLINE_CURVE_WITH_KNOTS ( ( 3, 2, 2, 2, 3 ),
 ( 0.7884615384615384359, 0.7948717948717948234, 0.8076923076923077094, 0.8205128205128204844, 0.8269230769230769829 ),
 .UNSPECIFIED. ) 
 CURVE ( )  GEOMETRIC_REPRESENTATION_ITEM ( )  RATIONAL_B_SPLINE_CURVE ( ( 0.9330127018922194093, 0.9330127018922194093, 1.000000000000000000, 0.8660254037844387076, 1.000000000000000000, 0.8660254037844387076, 1.000000000000000000, 0.9330127018922187432, 0.9330127018922192983 ) ) 
 REPRESENTATION_ITEM ( '' )  );
#10269 = CARTESIAN_POINT ( 'NONE',  ( -45.50000000000000000, -16.03270077640482683, -2.787981825772258837 ) ) ;
#10270 = CARTESIAN_POINT ( 'NONE',  ( -8.874038404635921751, 3.391377654146875642, -2.000000000000000000 ) ) ;
#10271 = CARTESIAN_POINT ( 'NONE',  ( -4.000000000000000000, -2.309401076758508253, -4.700000000000000178 ) ) ;
#10272 = CARTESIAN_POINT ( 'NONE',  ( 41.45058359766582612, -3.639327173243837255, -4.757684611182616763 ) ) ;
#10273 = EDGE_CURVE ( 'NONE', #7301, #8853, #6144, .T. ) ;
#10274 = CARTESIAN_POINT ( 'NONE',  ( 28.58911057998038530, -6.046239229258517867, -3.283357778048667797 ) ) ;
#10275 = CARTESIAN_POINT ( 'NONE',  ( -2.449848172108561428, -3.432307619358749395, -3.203702292528910700 ) ) ;
#10276 = CONTEXT_DEPENDENT_SHAPE_REPRESENTATION ( #1708, #2750 ) ;
#10277 = PLANE ( 'NONE',  #10662 ) ;
#10278 = CARTESIAN_POINT ( 'NONE',  ( 28.89355063163679915, -2.047864499088824175, -5.783357778048658027 ) ) ;
#10279 = CARTESIAN_POINT ( 'NONE',  ( 38.64694918415791136, -1.054552983374778208, -9.283357778048653586 ) ) ;
#10280 = CARTESIAN_POINT ( 'NONE',  ( 32.96459815279162342, -1.884545423566157174, 7.033357778048666020 ) ) ;
#10281 = CARTESIAN_POINT ( 'NONE',  ( 27.00222791626931595, -2.275731535614434531, 5.783357778048668685 ) ) ;
#10282 = EDGE_CURVE ( 'NONE', #963, #12549, #2056, .T. ) ;
#10283 = EDGE_LOOP ( 'NONE', ( #11855, #2928, #12924, #1338 ) ) ;
#10284 = CARTESIAN_POINT ( 'NONE',  ( 26.34117031759772942, -2.982346454214467535, -4.705209693361161349 ) ) ;
#10285 = VERTEX_POINT ( 'NONE', #4955 ) ;
#10286 = CARTESIAN_POINT ( 'NONE',  ( 26.46816385032927599, -3.594016774262162706, 7.939653947423664704 ) ) ;
#10287 = CARTESIAN_POINT ( 'NONE',  ( 27.50829672905005907, -3.268828784122926212, 8.283357778048666020 ) ) ;
#10288 = CYLINDRICAL_SURFACE ( 'NONE', #4419, 2.499999999999999112 ) ;
#10289 = ORIENTED_EDGE ( 'NONE', *, *, #6823, .F. ) ;
#10290 = CARTESIAN_POINT ( 'NONE',  ( 25.90934487712385348, 0.1208734971681838660, -5.783357778048663356 ) ) ;
#10291 = ORIENTED_EDGE ( 'NONE', *, *, #11694, .F. ) ;
#10292 = DIRECTION ( 'NONE',  ( -1.000000000000000000, 0.000000000000000000, 0.000000000000000000 ) ) ;
#10293 = DIRECTION ( 'NONE',  ( 0.000000000000000000, 0.000000000000000000, 1.000000000000000000 ) ) ;
#10294 = CARTESIAN_POINT ( 'NONE',  ( 33.13163345120441505, -4.045141346131868154, -3.627061608673664672 ) ) ;
#10295 = CARTESIAN_POINT ( 'NONE',  ( 25.84216048658649001, -4.923378882637265974, -3.283357778048664688 ) ) ;
#10296 = CARTESIAN_POINT ( 'NONE',  ( 0.000000000000000000, 0.000000000000000000, -1.901951201008075243 ) ) ;
#10297 = PLANE ( 'NONE',  #15922 ) ;
#10298 = CARTESIAN_POINT ( 'NONE',  ( 28.36401332423200827, -6.500457016816879374, -6.861505862736166250 ) ) ;
#10299 = LINE ( 'NONE', #16133, #10429 ) ;
#10300 = CARTESIAN_POINT ( 'NONE',  ( 33.14105852333657509, -6.224726188408045147, 7.033357778048657138 ) ) ;
#10301 = ORIENTED_EDGE ( 'NONE', *, *, #7175, .F. ) ;
#10302 = ORIENTED_EDGE ( 'NONE', *, *, #8574, .T. ) ;
#10303 = ORIENTED_EDGE ( 'NONE', *, *, #14347, .T. ) ;
#10304 = EDGE_CURVE ( 'NONE', #12046, #4105, #16989, .T. ) ;
#10305 = CARTESIAN_POINT ( 'NONE',  ( 27.24942365487322959, -6.207645047004940686, 8.283357778048660691 ) ) ;
#10306 = DIRECTION ( 'NONE',  ( 1.000000000000000000, 0.000000000000000000, 0.000000000000000000 ) ) ;
#10307 = FILL_AREA_STYLE ('',( #718 ) ) ;
#10308 = DIRECTION ( 'NONE',  ( 0.000000000000000000, 0.000000000000000000, 1.000000000000000000 ) ) ;
#10309 = CARTESIAN_POINT ( 'NONE',  ( -24.62400252878131113, -22.25686381702613659, -14.56428162264008286 ) ) ;
#10310 = CARTESIAN_POINT ( 'NONE',  ( 31.55553118839817728, -4.235030543236534939, -7.939653947423662039 ) ) ;
#10311 = CARTESIAN_POINT ( 'NONE',  ( 31.03132594549780876, -1.780107929003061473, -6.453230759126465266 ) ) ;
#10312 = DIRECTION ( 'NONE',  ( 0.000000000000000000, 0.000000000000000000, 1.000000000000000000 ) ) ;
#10313 = DIRECTION ( 'NONE',  ( -0.000000000000000000, -0.000000000000000000, -1.000000000000000000 ) ) ;
#10314 = DIRECTION ( 'NONE',  ( -1.000000000000000000, -0.000000000000000000, -0.000000000000000000 ) ) ;
#10315 = EDGE_CURVE ( 'NONE', #11675, #5034, #17528, .T. ) ;
#10316 = CARTESIAN_POINT ( 'NONE',  ( 27.84978555093622177, -3.227686124957687586, -8.283357778048660691 ) ) ;
#10317 = EDGE_LOOP ( 'NONE', ( #17218, #7152, #9834, #7474 ) ) ;
#10318 = CARTESIAN_POINT ( 'NONE',  ( 33.32855701603872234, -2.140504347050403045, -6.861505862736158257 ) ) ;
#10319 = CARTESIAN_POINT ( 'NONE',  ( -13.00000000000000178, 1.592040838891559293E-15, -6.000000000000000000 ) ) ;
#10320 = EDGE_LOOP ( 'NONE', ( #4801, #16544, #17049, #13242 ) ) ;
#10321 = ORIENTED_EDGE ( 'NONE', *, *, #6917, .F. ) ;
#10322 = DIRECTION ( 'NONE',  ( 0.9928203230275510771, 0.1196152422706609902, 4.006172263299092517E-17 ) ) ;
#10323 = CARTESIAN_POINT ( 'NONE',  ( 29.77118727536320719, -5.903822331637461396, 8.283357778048658915 ) ) ;
#10324 = CIRCLE ( 'NONE', #17323, 0.8999999999999998002 ) ;
#10325 = ORIENTED_EDGE ( 'NONE', *, *, #8159, .T. ) ;
#10326 = EDGE_CURVE ( 'NONE', #9479, #15536, #13131, .T. ) ;
#10327 = CARTESIAN_POINT ( 'NONE',  ( 4.000000000000000888, 0.9868501483902626381, -0.09357334158579776184 ) ) ;
#10328 = EDGE_CURVE ( 'NONE', #10789, #3948, #10142, .T. ) ;
#10329 = CARTESIAN_POINT ( 'NONE',  ( 32.04158527077989760, -6.057382223572642665, -4.705209693361168455 ) ) ;
#10330 = EDGE_LOOP ( 'NONE', ( #13202, #799 ) ) ;
#10331 = CARTESIAN_POINT ( 'NONE',  ( -31.74999999999995737, 0.000000000000000000, 0.000000000000000000 ) ) ;
#10332 = CARTESIAN_POINT ( 'NONE',  ( 25.76775864925888015, -2.837585720338237749, -6.439571894700457655 ) ) ;
#10333 = VERTEX_POINT ( 'NONE', #9140 ) ;
#10334 = PRODUCT_DEFINITION_FORMATION_WITH_SPECIFIED_SOURCE ( 'ANY', '', #13747, .NOT_KNOWN. ) ;
#10335 = FACE_OUTER_BOUND ( 'NONE', #10320, .T. ) ;
#10336 = ORIENTED_EDGE ( 'NONE', *, *, #1937, .T. ) ;
#10337 = CARTESIAN_POINT ( 'NONE',  ( 33.73390066541284682, -2.518766455766909385, -3.283357778048662023 ) ) ;
#10338 =( BOUNDED_CURVE ( )  B_SPLINE_CURVE ( 2, ( #15629, #7297, #1951, #670, #7565, #15728, #13091, #3303, #6282 ),
 .UNSPECIFIED., .F., .F. ) 
 B_SPLINE_CURVE_WITH_KNOTS ( ( 3, 2, 2, 2, 3 ),
 ( 0.3269230769230769273, 0.3333333333333333148, 0.3461538461538461453, 0.3589743589743589758, 0.3653846153846154188 ),
 .UNSPECIFIED. ) 
 CURVE ( )  GEOMETRIC_REPRESENTATION_ITEM ( )  RATIONAL_B_SPLINE_CURVE ( ( 0.9330127018922194093, 0.9330127018922194093, 1.000000000000000000, 0.8660254037844387076, 1.000000000000000000, 0.8660254037844387076, 1.000000000000000000, 0.9330127018922190762, 0.9330127018922194093 ) ) 
 REPRESENTATION_ITEM ( '' )  );
#10339 = VECTOR ( 'NONE', #8831, 1000.000000000000227 ) ;
#10340 = VERTEX_POINT ( 'NONE', #14679 ) ;
#10341 = CARTESIAN_POINT ( 'NONE',  ( 28.36401332423200827, -6.500457016816879374, -6.861505862736166250 ) ) ;
#10342 = LINE ( 'NONE', #15895, #5238 ) ;
#10343 = CARTESIAN_POINT ( 'NONE',  ( 27.16987539990068612, -2.245336462116964249, -6.453230759126464378 ) ) ;
#10344 = CARTESIAN_POINT ( 'NONE',  ( 0.000000000000000000, 0.000000000000000000, -8.700000000000001066 ) ) ;
#10345 = CARTESIAN_POINT ( 'NONE',  ( 29.18195272205665347, -2.340279496617377664, -4.533357778048659803 ) ) ;
#10346 = DIRECTION ( 'NONE',  ( 0.9928203230275512992, 0.1196152422706610180, 4.006172263299093133E-17 ) ) ;
#10347 = EDGE_CURVE ( 'NONE', #8806, #5050, #12179, .T. ) ;
#10348 = ADVANCED_FACE ( 'NONE', ( #10394 ), #11001, .F. ) ;
#10349 = AXIS2_PLACEMENT_3D ( 'NONE', #8249, #2727, #1449 ) ;
#10350 = ORIENTED_EDGE ( 'NONE', *, *, #14140, .T. ) ;
#10351 = DIRECTION ( 'NONE',  ( -0.000000000000000000, -0.000000000000000000, 1.000000000000000000 ) ) ;
#10352 = DIRECTION ( 'NONE',  ( 0.000000000000000000, 0.000000000000000000, -1.000000000000000000 ) ) ;
#10353 = CARTESIAN_POINT ( 'NONE',  ( 27.19802975513453092, -2.241944418315925613, 5.783357778048667797 ) ) ;
#10354 = ORIENTED_EDGE ( 'NONE', *, *, #1656, .T. ) ;
#10355 = DIRECTION ( 'NONE',  ( -0.06446199418653550395, -0.9979201627913403261, -4.248110196704583871E-22 ) ) ;
#10356 = DIRECTION ( 'NONE',  ( 0.000000000000000000, 0.000000000000000000, 1.000000000000000000 ) ) ;
#10357 = CARTESIAN_POINT ( 'NONE',  ( 31.89397184978405519, -6.712334120981523711, -5.783357778048663356 ) ) ;
#10358 = CARTESIAN_POINT ( 'NONE',  ( 15.92260893619738837, -28.39189527176317540, -16.15082599432113142 ) ) ;
#10359 = EDGE_CURVE ( 'NONE', #10285, #11171, #17946, .T. ) ;
#10360 =( BOUNDED_CURVE ( )  B_SPLINE_CURVE ( 2, ( #9078, #14526, #733, #14703, #8242, #15135, #2721 ),
 .UNSPECIFIED., .F., .F. ) 
 B_SPLINE_CURVE_WITH_KNOTS ( ( 3, 2, 2, 3 ),
 ( 0.9423076923076922906, 0.9487179487179486781, 0.9615384615384615641, 0.9690340935984054216 ),
 .UNSPECIFIED. ) 
 CURVE ( )  GEOMETRIC_REPRESENTATION_ITEM ( )  RATIONAL_B_SPLINE_CURVE ( ( 0.9330127018922194093, 0.9330127018922194093, 1.000000000000000000, 0.8660254037844387076, 1.000000000000000000, 0.9216705062683109295, 0.9349331465915117212 ) ) 
 REPRESENTATION_ITEM ( '' )  );
#10361 = CARTESIAN_POINT ( 'NONE',  ( 28.99436501219896201, -4.543600488427916417, -3.283357778048664688 ) ) ;
#10362 = DIRECTION ( 'NONE',  ( 0.9928203230275512992, 0.1196152422706610180, 4.006172263299093133E-17 ) ) ;
#10363 = DIRECTION ( 'NONE',  ( 1.000000000000000000, 0.000000000000000000, 0.000000000000000000 ) ) ;
#10364 = CARTESIAN_POINT ( 'NONE',  ( 30.81132015408399027, -5.578634341498224458, -3.627061608673668225 ) ) ;
#10365 = AXIS2_PLACEMENT_3D ( 'NONE', #7968, #2613, #17706 ) ;
#10366 = CARTESIAN_POINT ( 'NONE',  ( 25.11802603177690330, -19.03270077640482683, 10.53798182577225084 ) ) ;
#10368 = AXIS2_PLACEMENT_3D ( 'NONE', #10098, #688, #13012 ) ;
#10367 = CARTESIAN_POINT ( 'NONE',  ( 31.07327543742414022, -2.112412460091767308, -4.533357778048659803 ) ) ;
#10369 = CARTESIAN_POINT ( 'NONE',  ( 25.78518620311324838, -3.676302093007511651, 3.627061608673666893 ) ) ;
#10370 = ORIENTED_EDGE ( 'NONE', *, *, #6215, .F. ) ;
#10371 = B_SPLINE_CURVE_WITH_KNOTS ( 'NONE', 1,
 ( #13334, #2201 ),
 .UNSPECIFIED., .F., .F.,
 ( 2, 2 ),
 ( 0.000000000000000000, 1.000000000000000000 ),
 .UNSPECIFIED. ) ;
#10372 = ORIENTED_EDGE ( 'NONE', *, *, #2220, .F. ) ;
#10373 = CARTESIAN_POINT ( 'NONE',  ( 26.11428532722776907, -5.713797161519016399, 7.898105917008066079 ) ) ;
#10374 = EDGE_CURVE ( 'NONE', #11271, #11309, #9862, .T. ) ;
#10375 = ORIENTED_EDGE ( 'NONE', *, *, #13725, .F. ) ;
#10376 = CARTESIAN_POINT ( 'NONE',  ( 25.77727992838053339, -5.625024813964539128, 3.627061608673662896 ) ) ;
#10377 = CARTESIAN_POINT ( 'NONE',  ( -21.42089235853292806, -10.15736413759261048, 15.24668633003922658 ) ) ;
#10378 = CARTESIAN_POINT ( 'NONE',  ( 27.16987539990068612, -2.245336462116964249, -6.453230759126464378 ) ) ;
#10379 = VERTEX_POINT ( 'NONE', #17868 ) ;
#10380 = CYLINDRICAL_SURFACE ( 'NONE', #1863, 10.50000000000000000 ) ;
#10381 = AXIS2_PLACEMENT_3D ( 'NONE', #6715, #9348, #17737 ) ;
#10382 = CARTESIAN_POINT ( 'NONE',  ( -34.91600907648203389, -11.88801210197604341, -0.000000000000000000 ) ) ;
#10383 = VERTEX_POINT ( 'NONE', #5390 ) ;
#10384 = CARTESIAN_POINT ( 'NONE',  ( 2.500000000000000000, -1.178949249685213863, 2.042000000000001148 ) ) ;
#10385 = CARTESIAN_POINT ( 'NONE',  ( -23.00000000000000000, -16.21813761408365195, 13.00000000000000355 ) ) ;
#10386 = EDGE_CURVE ( 'NONE', #17484, #16733, #8220, .T. ) ;
#10387 = CARTESIAN_POINT ( 'NONE',  ( 30.76748005699505129, -4.329975141788874993, -7.939653947423662039 ) ) ;
#10388 = DIRECTION ( 'NONE',  ( 0.9928203230275512992, 0.1196152422706610180, 4.006172263299093133E-17 ) ) ;
#10389 = CARTESIAN_POINT ( 'NONE',  ( -8.632250723006720250, -18.84644399697197770, -13.00000000000000178 ) ) ;
#10390 = SURFACE_STYLE_USAGE ( .BOTH. , #4861 ) ;
#10391 = CARTESIAN_POINT ( 'NONE',  ( 26.47269060886452507, -6.728324053342490174, -6.861505862736166250 ) ) ;
#10392 = AXIS2_PLACEMENT_3D ( 'NONE', #7013, #15174, #1665 ) ;
#10393 = PRODUCT_DEFINITION_SHAPE ( 'NONE', 'NONE',  #17984 ) ;
#10394 = FACE_OUTER_BOUND ( 'NONE', #1764, .T. ) ;
#10395 = CARTESIAN_POINT ( 'NONE',  ( 31.74131510559286085, -5.666460835049168310, 8.283357778048658915 ) ) ;
#10396 = VECTOR ( 'NONE', #1726, 1000.000000000000114 ) ;
#10397 = ORIENTED_EDGE ( 'NONE', *, *, #8326, .T. ) ;
#10398 = EDGE_LOOP ( 'NONE', ( #2770, #7593, #5353, #519 ) ) ;
#10399 = ADVANCED_FACE ( 'NONE', ( #16475 ), #2642, .T. ) ;
#10400 = ORIENTED_EDGE ( 'NONE', *, *, #10044, .F. ) ;
#10401 = CARTESIAN_POINT ( 'NONE',  ( 26.25801688195511474, -3.619335333876111171, 3.627061608673666449 ) ) ;
#10402 = VECTOR ( 'NONE', #9001, 1000.000000000000227 ) ;
#10403 = CARTESIAN_POINT ( 'NONE',  ( 33.58707084003705745, -6.498152266226124851, 5.783357778048657138 ) ) ;
#10404 = ORIENTED_EDGE ( 'NONE', *, *, #2109, .F. ) ;
#10405 = CARTESIAN_POINT ( 'NONE',  ( 0.000000000000000000, 0.000000000000000000, -9.600000000000001421 ) ) ;
#10406 = DIRECTION ( 'NONE',  ( -0.000000000000000000, -0.000000000000000000, -1.000000000000000000 ) ) ;
#10407 = CARTESIAN_POINT ( 'NONE',  ( -18.90235488073503944, -20.95521764957430122, -15.70196361584510392 ) ) ;
#10408 = CARTESIAN_POINT ( 'NONE',  ( 27.86926259684567597, -5.933094176093606897, -7.939653947423664704 ) ) ;
#10409 = LINE ( 'NONE', #14610, #2655 ) ;
#10410 = LINE ( 'NONE', #11587, #16838 ) ;
#10411 = DIRECTION ( 'NONE',  ( -0.7681011886108269904, 0.5760758914581205481, -0.2795659695588259552 ) ) ;
#10412 = CARTESIAN_POINT ( 'NONE',  ( 26.31175009776946538, -7.352777558617343168, -6.181997573440047411 ) ) ;
#10413 = CARTESIAN_POINT ( 'NONE',  ( -20.00000000000000000, 7.999999999999996447, 15.51150668642334374 ) ) ;
#10414 = ORIENTED_EDGE ( 'NONE', *, *, #16354, .F. ) ;
#10415 = EDGE_CURVE ( 'NONE', #2179, #5245, #12476, .T. ) ;
#10416 = CARTESIAN_POINT ( 'NONE',  ( 26.23609683341064525, -2.995005734021441768, -6.861505862736159145 ) ) ;
#10417 = CARTESIAN_POINT ( 'NONE',  ( 31.41531425212677675, -1.744041783721344219, -5.783357778048658915 ) ) ;
#10418 = ORIENTED_EDGE ( 'NONE', *, *, #10531, .T. ) ;
#10419 = CARTESIAN_POINT ( 'NONE',  ( 2.687328764639639544, -3.067272167851296416, -0.05923475698271170320 ) ) ;
#10420 = CLOSED_SHELL ( 'NONE', ( #8130, #8300, #75, #7140, #1111, #7860, #2450, #13546, #1157, #8545, #2323, #11140, #17492, #14873, #13867, #7625, #13408, #11710, #13464, #127, #1064, #10909, #4464, #12719, #3396, #7165, #1333, #5233, #14264, #11776, #9314, #2333, #14748, #3970, #14676, #8432, #11355, #2810, #4318, #15148, #13585, #16449, #6236, #10198, #8936, #12623, #5237, #5079, #14010, #17838, #1253, #1286, #9019, #6941, #9277, #13394, #498, #3311, #4340, #3763, #13878, #12469, #11559, #15001, #5117, #13614, #14042, #12293, #13695, #14188, #10023, #6591, #4246, #326, #9406, #9956, #15886, #9502, #9920, #7896, #1878, #5784, #8304, #10812, #6515, #17332, #14632, #5665, #13905, #4083, #11873, #4890, #2133, #5880, #15494, #11858, #3847, #5109, #6475, #15271, #9336, #14615, #8868, #8679, #6038, #5916 ) ) ;
#10421 = ORIENTED_EDGE ( 'NONE', *, *, #14584, .T. ) ;
#10422 = CARTESIAN_POINT ( 'NONE',  ( 33.00219691583784964, -5.514549477365426888, -3.283357778048667797 ) ) ;
#10423 = CARTESIAN_POINT ( 'NONE',  ( 33.17094678975809074, -2.159493266760871499, -6.861505862736159145 ) ) ;
#10424 = ORIENTED_EDGE ( 'NONE', *, *, #837, .T. ) ;
#10425 = FACE_BOUND ( 'NONE', #14920, .T. ) ;
#10426 = STYLED_ITEM ( 'NONE', ( #9989 ), #11551 ) ;
#10427 = CARTESIAN_POINT ( 'NONE',  ( 31.12210306526553083, -4.287250072544045665, -8.283357778048662468 ) ) ;
#10428 = LINE ( 'NONE', #4726, #6956 ) ;
#10429 = VECTOR ( 'NONE', #3516, 1000.000000000000227 ) ;
#10430 = CARTESIAN_POINT ( 'NONE',  ( -0.02448804030507887100, -4.877043185438137307, -3.451162025751992157 ) ) ;
#10431 = CARTESIAN_POINT ( 'NONE',  ( 30.33776104811456165, -2.201027418740610919, -7.033357778048658027 ) ) ;
#10432 = CLOSED_SHELL ( 'NONE', ( #3367, #8882, #15490, #3802, #1936, #1600, #2076, #13715, #4738, #15899, #1240, #10933, #13157, #2308, #8292, #9097, #915, #14698, #10252, #5727, #13864, #6172, #388, #7814, #4734, #12210, #15925, #14128, #13975, #7959, #14536, #9428, #10160, #6205, #8023, #5508, #15826, #12335, #12930, #10079, #8459, #2988, #15848, #1668 ) ) ;
#10433 = ADVANCED_FACE ( 'NONE', ( #8301 ), #12380, .F. ) ;
#10434 = MECHANICAL_DESIGN_GEOMETRIC_PRESENTATION_REPRESENTATION (  '', ( #15961 ), #15076 ) ;
#10435 = CARTESIAN_POINT ( 'NONE',  ( 26.97161122272022382, -2.906390775372597712, -4.705209693361161349 ) ) ;
#10436 = CARTESIAN_POINT ( 'NONE',  ( 26.04653150877178902, -5.151432644682725659, -3.575219446611406227 ) ) ;
#10437 = FACE_OUTER_BOUND ( 'NONE', #10802, .T. ) ;
#10438 = CARTESIAN_POINT ( 'NONE',  ( 6.540214080563054644, 17.14393242671841477, -16.94648454462088694 ) ) ;
#10439 = CARTESIAN_POINT ( 'NONE',  ( 29.23078034989804763, -4.515117109069654688, -8.283357778048662468 ) ) ;
#10440 = CARTESIAN_POINT ( 'NONE',  ( 31.25770402584614871, -1.763030703431812451, -5.783357778048658915 ) ) ;
#10441 = VECTOR ( 'NONE', #14795, 1000.000000000000000 ) ;
#10442 = EDGE_LOOP ( 'NONE', ( #7334, #195, #10699, #7519 ) ) ;
#10443 = LINE ( 'NONE', #16003, #10339 ) ;
#10444 = CARTESIAN_POINT ( 'NONE',  ( 26.78782184427022983, -4.809445364374452581, -8.283357778048662468 ) ) ;
#10445 = CARTESIAN_POINT ( 'NONE',  ( -1.312671235360379107, -3.860931062424225235, -0.05923475698271177259 ) ) ;
#10446 = ORIENTED_EDGE ( 'NONE', *, *, #1996, .T. ) ;
#10447 = LINE ( 'NONE', #6555, #16904 ) ;
#10448 =( BOUNDED_CURVE ( )  B_SPLINE_CURVE ( 2, ( #5932, #597, #17023, #4840, #1883, #11456, #10280, #4931, #15647 ),
 .UNSPECIFIED., .F., .T. ) 
 B_SPLINE_CURVE_WITH_KNOTS ( ( 3, 2, 2, 2, 3 ),
 ( 0.05769230769230772327, 0.06410256410256409687, 0.07692307692307692735, 0.08974358974358974395, 0.09615384615384617306 ),
 .UNSPECIFIED. ) 
 CURVE ( )  GEOMETRIC_REPRESENTATION_ITEM ( )  RATIONAL_B_SPLINE_CURVE ( ( 0.9330127018922192983, 0.9330127018922196314, 1.000000000000000000, 0.8660254037844387076, 1.000000000000000000, 0.8660254037844387076, 1.000000000000000000, 0.9330127018922191873, 0.9330127018922194093 ) ) 
 REPRESENTATION_ITEM ( '' )  );
#10449 = LINE ( 'NONE', #5856, #13077 ) ;
#10450 = CARTESIAN_POINT ( 'NONE',  ( 25.95642634701329499, -4.403549397486667516, -3.686412874245489135 ) ) ;
#10451 = CARTESIAN_POINT ( 'NONE',  ( 31.66930131758986633, -2.967382423816733894, -3.627061608673662008 ) ) ;
#10452 = LINE ( 'NONE', #16103, #10502 ) ;
#10453 = AXIS2_PLACEMENT_3D ( 'NONE', #4675, #514, #1698 ) ;
#10454 = ADVANCED_FACE ( 'NONE', ( #8127 ), #297, .F. ) ;
#10455 = CARTESIAN_POINT ( 'NONE',  ( 27.86101441917510257, -1.772519683195811657, -5.783357778048658027 ) ) ;
#10456 = CYLINDRICAL_SURFACE ( 'NONE', #2611, 2.500000000000001776 ) ;
#10457 = EDGE_CURVE ( 'NONE', #15335, #3112, #7805, .T. ) ;
#10458 = CONTEXT_DEPENDENT_SHAPE_REPRESENTATION ( #3452, #12438 ) ;
#10459 = CARTESIAN_POINT ( 'NONE',  ( 29.25000000000000000, -16.21813761408365195, -13.00000000000000178 ) ) ;
#10460 = CARTESIAN_POINT ( 'NONE',  ( 11.38175538881591287, -22.33742387525453665, -16.67884400577319681 ) ) ;
#10461 = CARTESIAN_POINT ( 'NONE',  ( 29.67743187657054449, -6.342216019229654833, -4.705209693361169343 ) ) ;
#10462 = AXIS2_PLACEMENT_3D ( 'NONE', #11037, #12054, #10679 ) ;
#10463 = CARTESIAN_POINT ( 'NONE',  ( 27.65467808709180630, -4.705006306174339237, -3.283357778048664688 ) ) ;
#10464 = CARTESIAN_POINT ( 'NONE',  ( 31.89397184978405519, -6.712334120981523711, -5.783357778048663356 ) ) ;
#10465 = CARTESIAN_POINT ( 'NONE',  ( 27.25621498173240198, -3.499072175709823984, 7.939653947423664704 ) ) ;
#10466 = ORIENTED_EDGE ( 'NONE', *, *, #8612, .F. ) ;
#10467 = CARTESIAN_POINT ( 'NONE',  ( 32.29220775574281532, -1.628196571319322050, -6.453230759126467042 ) ) ;
#10468 = VERTEX_POINT ( 'NONE', #2536 ) ;
#10469 = CARTESIAN_POINT ( 'NONE',  ( 32.72003615946069743, -2.840789625746940938, 3.627061608673666893 ) ) ;
#10470 = CARTESIAN_POINT ( 'NONE',  ( 28.16197717867739314, -7.161965777771100328, 6.453230759126468818 ) ) ;
#10471 = ORIENTED_EDGE ( 'NONE', *, *, #10958, .T. ) ;
#10472 = CARTESIAN_POINT ( 'NONE',  ( 4.000000000000000000, -0.7890432684750885439, -0.04868663549882413372 ) ) ;
#10473 = CIRCLE ( 'NONE', #3540, 10.50000000000000000 ) ;
#10474 = DIRECTION ( 'NONE',  ( 0.000000000000000000, 0.8660254037844380415, -0.5000000000000009992 ) ) ;
#10475 = DIRECTION ( 'NONE',  ( -1.000000000000000000, -0.000000000000000000, -0.000000000000000000 ) ) ;
#10476 = CARTESIAN_POINT ( 'NONE',  ( 33.56515079149260572, -5.873822666371450119, -6.861505862736167138 ) ) ;
#10477 = CARTESIAN_POINT ( 'NONE',  ( 31.53813789838894621, -6.745008222462202774, -5.783357778048668685 ) ) ;
#10478 = CARTESIAN_POINT ( 'NONE',  ( -1.257202807338834605, 3.892955774274010849, -3.133250573521422222 ) ) ;
#10479 = CIRCLE ( 'NONE', #8176, 2.499999999999999556 ) ;
#10480 = DIRECTION ( 'NONE',  ( 0.9928203230275510771, 0.1196152422706614621, -0.000000000000000000 ) ) ;
#10481 = CARTESIAN_POINT ( 'NONE',  ( 28.25893984004492765, -6.513116296623863377, -4.705209693361168455 ) ) ;
#10482 = APPLICATION_CONTEXT ( 'automotive_design' ) ;
#10483 = EDGE_CURVE ( 'NONE', #1653, #7229, #11607, .T. ) ;
#10484 = CARTESIAN_POINT ( 'NONE',  ( 34.91600907648203389, -11.88801210197604341, 11.56671555609732671 ) ) ;
#10485 = CARTESIAN_POINT ( 'NONE',  ( 26.23123039439649062, -6.684454722870800225, -4.255767710538254534 ) ) ;
#10486 = DIRECTION ( 'NONE',  ( -0.4714752725849062909, -0.8818792816145463176, -1.010345934383541768E-15 ) ) ;
#10487 = VECTOR ( 'NONE', #15737, 1000.000000000000114 ) ;
#10488 = AXIS2_PLACEMENT_3D ( 'NONE', #15600, #382, #468 ) ;
#10489 = CARTESIAN_POINT ( 'NONE',  ( 33.09223089549517738, -4.049888575955752579, 3.283357778048664244 ) ) ;
#10490 = VECTOR ( 'NONE', #15888, 1000.000000000000114 ) ;
#10491 = ORIENTED_EDGE ( 'NONE', *, *, #4788, .T. ) ;
#10492 = ORIENTED_EDGE ( 'NONE', *, *, #13199, .F. ) ;
#10493 = EDGE_LOOP ( 'NONE', ( #4334, #14303, #5708 ) ) ;
#10494 = CARTESIAN_POINT ( 'NONE',  ( 35.62429925076629189, -17.76690233603958546, 10.53798182577225084 ) ) ;
#10495 = CARTESIAN_POINT ( 'NONE',  ( 32.28234893270314387, -5.401404424200516807, 3.627061608673662896 ) ) ;
#10496 = ORIENTED_EDGE ( 'NONE', *, *, #12537, .F. ) ;
#10497 = CARTESIAN_POINT ( 'NONE',  ( 33.06225340847440464, -6.234220648470727433, 7.033357778048657138 ) ) ;
#10498 = CARTESIAN_POINT ( 'NONE',  ( 10.50000000000000000, 1.285879139104720831E-15, -4.000000000000000000 ) ) ;
#10499 = CARTESIAN_POINT ( 'NONE',  ( 30.28142597461332741, -2.507623461452779701, -4.705209693361160461 ) ) ;
#10500 = CARTESIAN_POINT ( 'NONE',  ( 30.33776104811456165, -2.201027418740610919, -7.033357778048658027 ) ) ;
#10501 = CARTESIAN_POINT ( 'NONE',  ( -36.27615609941022257, -23.17738945083361557, -0.000000000000000000 ) ) ;
#10502 = VECTOR ( 'NONE', #6203, 1000.000000000000000 ) ;
#10503 = FACE_BOUND ( 'NONE', #7695, .T. ) ;
#10504 = DIRECTION ( 'NONE',  ( -1.000000000000000000, 0.000000000000000000, 0.000000000000000000 ) ) ;
#10505 = CARTESIAN_POINT ( 'NONE',  ( 20.84129949943806537, -10.34926000617958231, 15.35708546568073984 ) ) ;
#10506 = SHAPE_REPRESENTATION_RELATIONSHIP ( 'NONE' , 'NONE' ,  #5639, #17227 ) ;
#10507 = EDGE_CURVE ( 'NONE', #14701, #4898, #10371, .T. ) ;
#10508 = CARTESIAN_POINT ( 'NONE',  ( 27.60205212784272177, -2.830435096530727446, -4.705209693361161349 ) ) ;
#10509 = CARTESIAN_POINT ( 'NONE',  ( 32.80318959510331212, -2.203800746085299522, -4.705209693361160461 ) ) ;
#10510 = ORIENTED_EDGE ( 'NONE', *, *, #7834, .F. ) ;
#10511 = CARTESIAN_POINT ( 'NONE',  ( 38.70301816123731697, -5.700001250565214228, -1.783357778048662690 ) ) ;
#10512 = CARTESIAN_POINT ( 'NONE',  ( 26.58890374069123652, -3.379597482641427231, 3.283357778048666464 ) ) ;
#10513 = EDGE_CURVE ( 'NONE', #15016, #13726, #5521, .T. ) ;
#10514 = VERTEX_POINT ( 'NONE', #13240 ) ;
#10515 = CARTESIAN_POINT ( 'NONE',  ( 4.000000000000000000, 0.7924765000094643463, -0.05906175389889926214 ) ) ;
#10516 = CARTESIAN_POINT ( 'NONE',  ( 31.49429780130001788, -5.496349022752856861, -7.939653947423662927 ) ) ;
#10517 = EDGE_LOOP ( 'NONE', ( #6568, #3601, #16591, #2311 ) ) ;
#10518 = EDGE_CURVE ( 'NONE', #7467, #133, #15377, .T. ) ;
#10519 = FACE_OUTER_BOUND ( 'NONE', #4694, .T. ) ;
#10520 = CARTESIAN_POINT ( 'NONE',  ( 28.71361296893772774, -7.095504558991913235, -5.113484796970856117 ) ) ;
#10521 = CARTESIAN_POINT ( 'NONE',  ( 8.632250723006720250, -18.84644399697197770, -13.00000000000000178 ) ) ;
#10522 = CIRCLE ( 'NONE', #7364, 13.00000000000000178 ) ;
#10523 = DIRECTION ( 'NONE',  ( -0.9979201627913402151, 0.06446199418653550395, 5.311609029246448998E-22 ) ) ;
#10524 = CARTESIAN_POINT ( 'NONE',  ( 32.50309786422735669, -5.574681056656012323, -8.283357778048662468 ) ) ;
#10525 = CARTESIAN_POINT ( 'NONE',  ( 25.83772294520678159, -3.669972453104032084, -3.627061608673662896 ) ) ;
#10526 = DIRECTION ( 'NONE',  ( 0.9928203230275510771, 0.1196152422706614621, -0.000000000000000000 ) ) ;
#10527 = DIRECTION ( 'NONE',  ( -0.9928203230275512992, -0.1196152422706610180, -4.006172263299093133E-17 ) ) ;
#10528 = CARTESIAN_POINT ( 'NONE',  ( 2.836862643238821313, 3.208966885971292538, -3.205052026701870282 ) ) ;
#10529 = CARTESIAN_POINT ( 'NONE',  ( 28.75424055680402802, -6.753251120556833520, -7.033357778048666908 ) ) ;
#10530 = CARTESIAN_POINT ( 'NONE',  ( 33.27602027394517847, -2.146833986953896822, -4.705209693361161349 ) ) ;
#10531 = EDGE_CURVE ( 'NONE', #4832, #14580, #8235, .T. ) ;
#10532 = EDGE_LOOP ( 'NONE', ( #6610, #17536, #4579, #171, #15264 ) ) ;
#10533 = FACE_OUTER_BOUND ( 'NONE', #6950, .T. ) ;
#10534 = CARTESIAN_POINT ( 'NONE',  ( -36.27615609941022257, -23.17738945083361202, -11.07596365154449636 ) ) ;
#10535 = DIRECTION ( 'NONE',  ( 1.000000000000000000, 0.000000000000000000, 0.000000000000000000 ) ) ;
#10536 = ORIENTED_EDGE ( 'NONE', *, *, #17702, .T. ) ;
#10537 = DIRECTION ( 'NONE',  ( 0.1196152422706596996, -0.9928203230275514102, 0.000000000000000000 ) ) ;
#10538 = DIRECTION ( 'NONE',  ( 0.000000000000000000, -1.000000000000000000, 3.469446951953614189E-16 ) ) ;
#10539 = CARTESIAN_POINT ( 'NONE',  ( 0.000000000000000000, 0.000000000000000000, 0.000000000000000000 ) ) ;
#10540 = EDGE_CURVE ( 'NONE', #9716, #757, #2927, .T. ) ;
#10541 = CARTESIAN_POINT ( 'NONE',  ( 29.39961944441754227, -3.040961747597316300, -3.283357778048662023 ) ) ;
#10542 = LINE ( 'NONE', #15823, #16805 ) ;
#10543 = CARTESIAN_POINT ( 'NONE',  ( 31.92212620501791775, -6.708942077180482855, 5.113484796970852564 ) ) ;
#10544 = CARTESIAN_POINT ( 'NONE',  ( 15.92260893619738837, -28.39189527176317540, -16.15082599432113142 ) ) ;
#10545 = VERTEX_POINT ( 'NONE', #4985 ) ;
#10546 = CARTESIAN_POINT ( 'NONE',  ( 29.76058531221316628, -5.705227139567997874, -7.939653947423664704 ) ) ;
#10547 = CARTESIAN_POINT ( 'NONE',  ( 0.000000000000000000, 0.000000000000000000, 8.700000000000001066 ) ) ;
#10548 = CARTESIAN_POINT ( 'NONE',  ( 29.45101334415624095, -7.006662376286321603, 5.783357778048669573 ) ) ;
#10549 = CARTESIAN_POINT ( 'NONE',  ( 26.19678349485696955, -4.880653813392439311, 7.939653947423662039 ) ) ;
#10550 = ORIENTED_EDGE ( 'NONE', *, *, #13991, .T. ) ;
#10551 = ORIENTED_EDGE ( 'NONE', *, *, #4228, .T. ) ;
#10552 = EDGE_CURVE ( 'NONE', #3859, #1701, #11967, .T. ) ;
#10553 = CARTESIAN_POINT ( 'NONE',  ( 28.51709679197739078, -3.347160818026084339, 7.939653947423664704 ) ) ;
#10554 = CARTESIAN_POINT ( 'NONE',  ( -4.000000000000000000, 2.309401076758501592, -4.700000000000000178 ) ) ;
#10555 = CARTESIAN_POINT ( 'NONE',  ( -4.211140560182196957, -2.431303136016548017, -3.445885042887436356 ) ) ;
#10556 = EDGE_CURVE ( 'NONE', #625, #11483, #11896, .T. ) ;
#10557 = ORIENTED_EDGE ( 'NONE', *, *, #1518, .T. ) ;
#10558 = CARTESIAN_POINT ( 'NONE',  ( -1.500000000000000222, -9.380831519646861238, -2.000000000000000000 ) ) ;
#10559 = CARTESIAN_POINT ( 'NONE',  ( -45.50000000000000000, -16.03270077640482683, 5.537981825772250843 ) ) ;
#10560 = CARTESIAN_POINT ( 'NONE',  ( 28.19013153391124860, -7.158573733970061248, -5.783357778048657138 ) ) ;
#10561 = CARTESIAN_POINT ( 'NONE',  ( 33.35047706458318828, -2.764833946905071560, -7.939653947423660263 ) ) ;
#10562 = CARTESIAN_POINT ( 'NONE',  ( 32.65880277236253448, -4.102108105263264193, -7.939653947423662039 ) ) ;
#10563 = AXIS2_PLACEMENT_3D ( 'NONE', #6933, #12466, #14928 ) ;
#10564 = CARTESIAN_POINT ( 'NONE',  ( -2.807096675500661664, 3.225959780909132490, -3.202509183706299112 ) ) ;
#10565 = FACE_BOUND ( 'NONE', #3159, .T. ) ;
#10566 = CARTESIAN_POINT ( 'NONE',  ( 28.75786045390062995, -2.691183018653962034, -6.861505862736159145 ) ) ;
#10567 = DIRECTION ( 'NONE',  ( 0.9928203230275510771, 0.1196152422706621282, 0.000000000000000000 ) ) ;
#10568 = DIRECTION ( 'NONE',  ( 0.7999999999999999334, -0.6000000000000001998, 0.000000000000000000 ) ) ;
#10569 = CARTESIAN_POINT ( 'NONE',  ( 31.70371634254663817, -2.036456781249897485, -4.533357778048659803 ) ) ;
#10570 = CARTESIAN_POINT ( 'NONE',  ( 28.72797218747911074, -6.756415940301135237, 7.033357778048657138 ) ) ;
#10571 = ORIENTED_EDGE ( 'NONE', *, *, #8693, .F. ) ;
#10572 = VERTEX_POINT ( 'NONE', #16074 ) ;
#10573 = CARTESIAN_POINT ( 'NONE',  ( 27.10313151398701947, -6.652368374500619908, 4.705209693361160461 ) ) ;
#10574 = CARTESIAN_POINT ( 'NONE',  ( 28.40332666278570173, -4.614808937445885384, 3.627061608673664228 ) ) ;
#10575 = VERTEX_POINT ( 'NONE', #10672 ) ;
#10576 = EDGE_CURVE ( 'NONE', #17612, #17698, #14874, .T. ) ;
#10577 = LINE ( 'NONE', #16144, #5751 ) ;
#10578 = CARTESIAN_POINT ( 'NONE',  ( 29.19631194059803292, -2.001190877926593004, -5.113484796970855228 ) ) ;
#10579 = CARTESIAN_POINT ( 'NONE',  ( 28.93739072872572393, -3.296523698798161650, -7.939653947423660263 ) ) ;
#10580 = DIRECTION ( 'NONE',  ( -1.000000000000000000, 0.000000000000000000, 0.000000000000000000 ) ) ;
#10581 = CARTESIAN_POINT ( 'NONE',  ( 33.18226487515251222, -2.585227674546096033, -3.283357778048662023 ) ) ;
#10582 = CARTESIAN_POINT ( 'NONE',  ( 0.000000000000000000, 0.000000000000000000, -3.000000000000002665 ) ) ;
#10583 = CARTESIAN_POINT ( 'NONE',  ( 26.49878054387835746, -2.963357534503999968, -4.705209693361160461 ) ) ;
#10584 = CARTESIAN_POINT ( 'NONE',  ( 23.84286890107044954, -10.01213378893004879, 14.74186762137086859 ) ) ;
#10585 = EDGE_CURVE ( 'NONE', #17331, #13453, #13924, .T. ) ;
#10586 = CARTESIAN_POINT ( 'NONE',  ( 31.06530721954707985, -6.801974981593605030, -5.783357778048669573 ) ) ;
#10587 = CARTESIAN_POINT ( 'NONE',  ( 31.66930131758986633, -2.967382423816733894, -3.627061608673662008 ) ) ;
#10588 = ORIENTED_EDGE ( 'NONE', *, *, #3067, .T. ) ;
#10589 = CARTESIAN_POINT ( 'NONE',  ( 1.746467850512308208E-21, -1.591841644184202181E-21, -6.005572809000082835 ) ) ;
#10590 = CARTESIAN_POINT ( 'NONE',  ( 0.000000000000000000, 0.000000000000000000, -3.000000000000002665 ) ) ;
#10591 = VERTEX_POINT ( 'NONE', #8064 ) ;
#10592 = CARTESIAN_POINT ( 'NONE',  ( 32.41296236253129592, -1.951006642345344044, -4.533357778048659803 ) ) ;
#10593 = CARTESIAN_POINT ( 'NONE',  ( 32.14213199643173624, -2.910415664685331638, -3.627061608673662896 ) ) ;
#10594 = EDGE_LOOP ( 'NONE', ( #15821, #2972, #6216, #8652 ) ) ;
#10595 = EDGE_CURVE ( 'NONE', #8691, #14539, #13600, .T. ) ;
#10596 = VERTEX_POINT ( 'NONE', #4891 ) ;
#10597 = CARTESIAN_POINT ( 'NONE',  ( -19.43845002722867221, 2.988003976273734263, 0.000000000000000000 ) ) ;
#10598 = CARTESIAN_POINT ( 'NONE',  ( 25.77386970449396841, -2.888308184441632953, -6.623114134516397300 ) ) ;
#10599 = CARTESIAN_POINT ( 'NONE',  ( 28.72797218747911074, -6.756415940301135237, -4.533357778048668685 ) ) ;
#10600 = CARTESIAN_POINT ( 'NONE',  ( -3.248936832696171617, 17.78798921770683350, 17.00000000000000000 ) ) ;
#10601 = CARTESIAN_POINT ( 'NONE',  ( 31.56485473504790917, -1.326280070207274564, -5.783357778048658027 ) ) ;
#10602 = EDGE_CURVE ( 'NONE', #1274, #1497, #2170, .T. ) ;
#10603 =( BOUNDED_CURVE ( )  B_SPLINE_CURVE ( 2, ( #16968, #8706, #14053, #10137, #12778, #9860, #15685, #15414, #11490 ),
 .UNSPECIFIED., .F., .T. ) 
 B_SPLINE_CURVE_WITH_KNOTS ( ( 3, 2, 2, 2, 3 ),
 ( 0.1730769230769231004, 0.1794871794871794879, 0.1923076923076923184, 0.2051282051282051211, 0.2115384615384615641 ),
 .UNSPECIFIED. ) 
 CURVE ( )  GEOMETRIC_REPRESENTATION_ITEM ( )  RATIONAL_B_SPLINE_CURVE ( ( 0.9330127018922194093, 0.9330127018922196314, 1.000000000000000000, 0.8660254037844387076, 1.000000000000000000, 0.8660254037844387076, 1.000000000000000000, 0.9330127018922190762, 0.9330127018922194093 ) ) 
 REPRESENTATION_ITEM ( '' )  );
#10604 = EDGE_LOOP ( 'NONE', ( #531, #11943 ) ) ;
#10605 = CARTESIAN_POINT ( 'NONE',  ( 32.77709966008947617, -5.968767264923789284, -6.861505862736166250 ) ) ;
#10606 = CARTESIAN_POINT ( 'NONE',  ( -30.07408527595751124, -27.82894256842315883, -13.18310524188696853 ) ) ;
#10607 = CARTESIAN_POINT ( 'NONE',  ( 3.035766082959412415E-15, 4.618802153517010289, -0.5000000000000000000 ) ) ;
#10608 = CARTESIAN_POINT ( 'NONE',  ( 3.248936832696173393, 17.78798921770683350, -17.00000000000000000 ) ) ;
#10609 = CARTESIAN_POINT ( 'NONE',  ( 29.74110826630370497, -2.999819088432076786, -8.283357778048658915 ) ) ;
#10610 = CARTESIAN_POINT ( 'NONE',  ( 30.86385689617753059, -5.572304701594727128, -7.939653947423662927 ) ) ;
#10611 = EDGE_LOOP ( 'NONE', ( #5195, #7534, #13407, #8039, #8834 ) ) ;
#10612 = CARTESIAN_POINT ( 'NONE',  ( 35.77680296528374271, -19.03270077640482683, 10.53798182577225084 ) ) ;
#10613 = CARTESIAN_POINT ( 'NONE',  ( 38.70301816123731697, -5.700001250565210675, -9.783357778048662468 ) ) ;
#10614 = ORIENTED_EDGE ( 'NONE', *, *, #686, .T. ) ;
#10615 = CARTESIAN_POINT ( 'NONE',  ( 27.48088551392658729, -7.244023872874614689, 5.783357778048669573 ) ) ;
#10616 = DIRECTION ( 'NONE',  ( 1.000000000000000000, 0.000000000000000000, 0.000000000000000000 ) ) ;
#10617 = CIRCLE ( 'NONE', #15261, 2.749999999999995559 ) ;
#10618 = CARTESIAN_POINT ( 'NONE',  ( 33.43363050022580296, -2.127845067243429256, -4.705209693361160461 ) ) ;
#10619 = CARTESIAN_POINT ( 'NONE',  ( -8.874038404635992805, -3.391377654146690013, -2.000000000000000000 ) ) ;
#10620 = CARTESIAN_POINT ( 'NONE',  ( 29.46348657678868577, -6.667800981652280967, -7.033357778048666908 ) ) ;
#10621 = CARTESIAN_POINT ( 'NONE',  ( -7.499998387031003411, -20.49508120620799900, -13.00000000000000178 ) ) ;
#10622 = LINE ( 'NONE', #8196, #8359 ) ;
#10623 = CARTESIAN_POINT ( 'NONE',  ( 0.000000000000000000, 0.000000000000000000, -10.47749643873921244 ) ) ;
#10624 = CARTESIAN_POINT ( 'NONE',  ( 30.91186687973582536, -2.431667782610909434, -4.705209693361160461 ) ) ;
#10625 = ADVANCED_FACE ( 'NONE', ( #1442 ), #13776, .T. ) ;
#10626 = CARTESIAN_POINT ( 'NONE',  ( 33.30246708102489350, -5.905470865888903020, -4.705209693361168455 ) ) ;
#10627 = CARTESIAN_POINT ( 'NONE',  ( 0.000000000000000000, 0.000000000000000000, -3.700000000000000178 ) ) ;
#10628 = CARTESIAN_POINT ( 'NONE',  ( 27.63266882139180680, -2.199775856772564708, 5.783357778048668685 ) ) ;
#10629 = VECTOR ( 'NONE', #7520, 1000.000000000000000 ) ;
#10630 = EDGE_LOOP ( 'NONE', ( #11292, #8722, #10303, #6470 ) ) ;
#10631 = CARTESIAN_POINT ( 'NONE',  ( 31.69574812466957781, -6.726019302751734763, 5.783357778048657138 ) ) ;
#10632 = DIRECTION ( 'NONE',  ( 0.000000000000000000, 0.000000000000000000, 1.000000000000000000 ) ) ;
#10633 = CARTESIAN_POINT ( 'NONE',  ( 35.74085044863416982, -23.57886868891565513, 11.27079897466147251 ) ) ;
#10634 = ORIENTED_EDGE ( 'NONE', *, *, #1946, .T. ) ;
#10635 = CARTESIAN_POINT ( 'NONE',  ( 33.16732689266149237, -6.221561368663743430, -7.033357778048666908 ) ) ;
#10636 = AXIS2_PLACEMENT_3D ( 'NONE', #17166, #4889, #11872 ) ;
#10637 = LINE ( 'NONE', #701, #2893 ) ;
#10638 = ORIENTED_EDGE ( 'NONE', *, *, #6111, .T. ) ;
#10639 = FACE_BOUND ( 'NONE', #11005, .T. ) ;
#10640 = DIRECTION ( 'NONE',  ( 0.000000000000000000, 0.000000000000000000, -1.000000000000000000 ) ) ;
#10641 = VECTOR ( 'NONE', #3746, 1000.000000000000114 ) ;
#10642 = CARTESIAN_POINT ( 'NONE',  ( 28.48022645605872327, -3.151730446115816875, -8.283357778048660691 ) ) ;
#10643 = CIRCLE ( 'NONE', #2840, 5.560781378645573980 ) ;
#10644 = CARTESIAN_POINT ( 'NONE',  ( 36.27615609941022257, -23.17738945083361557, -12.00000000000000000 ) ) ;
#10645 =( NAMED_UNIT ( * ) SI_UNIT ( $, .STERADIAN. ) SOLID_ANGLE_UNIT ( ) );
#10646 = CARTESIAN_POINT ( 'NONE',  ( 25.81099976294218479, -6.186279776075334524, 4.026415200706355613 ) ) ;
#10647 = EDGE_CURVE ( 'NONE', #11147, #17504, #3759, .T. ) ;
#10648 = DIRECTION ( 'NONE',  ( -0.1196152422706610735, 0.9928203230275511881, 0.000000000000000000 ) ) ;
#10649 = CARTESIAN_POINT ( 'NONE',  ( 32.22908376348204484, -1.973160382215000785, 4.533357778048667797 ) ) ;
#10650 = CARTESIAN_POINT ( 'NONE',  ( 32.26971135134834867, -1.630906943779925955, -5.113484796970855228 ) ) ;
#10651 = CARTESIAN_POINT ( 'NONE',  ( 27.29814976067589072, -3.294147343736873346, 3.283357778048666464 ) ) ;
#10652 = VERTEX_POINT ( 'NONE', #9582 ) ;
#10653 = ORIENTED_EDGE ( 'NONE', *, *, #9191, .F. ) ;
#10654 = CARTESIAN_POINT ( 'NONE',  ( 33.28924367748503244, -4.026152426421394814, 3.627061608673664228 ) ) ;
#10655 = CARTESIAN_POINT ( 'NONE',  ( 30.43486631442457835, -6.877930660435475296, 5.783357778048657138 ) ) ;
#10656 = EDGE_LOOP ( 'NONE', ( #14287, #1350, #9418, #11008 ) ) ;
#10657 = DIRECTION ( 'NONE',  ( 0.000000000000000000, 0.000000000000000000, 1.000000000000000000 ) ) ;
#10658 = DIRECTION ( 'NONE',  ( 0.000000000000000000, 0.000000000000000000, -1.000000000000000000 ) ) ;
#10659 = CARTESIAN_POINT ( 'NONE',  ( -11.73134587110777005, -4.864722402403119261, -9.600000000000001421 ) ) ;
#10660 = CARTESIAN_POINT ( 'NONE',  ( 28.49970350196817392, -5.857138497251738407, -7.939653947423664704 ) ) ;
#10661 = CARTESIAN_POINT ( 'NONE',  ( 0.000000000000000000, 0.000000000000000000, -12.00000000000000000 ) ) ;
#10662 = AXIS2_PLACEMENT_3D ( 'NONE', #14573, #6297, #16018 ) ;
#10663 = DIRECTION ( 'NONE',  ( 0.9928203230275510771, 0.1196152422706609902, 4.006172263299092517E-17 ) ) ;
#10664 = DIRECTION ( 'NONE',  ( 0.000000000000000000, 0.000000000000000000, 1.000000000000000000 ) ) ;
#10665 = CARTESIAN_POINT ( 'NONE',  ( 27.04606801335823718, -3.524390735323772006, -7.939653947423660263 ) ) ;
#10666 = CARTESIAN_POINT ( 'NONE',  ( -19.49912934580633106, 8.667827538924893105, 15.60122950519025409 ) ) ;
#10667 = AXIS2_PLACEMENT_3D ( 'NONE', #12939, #4685, #11472 ) ;
#10668 = CARTESIAN_POINT ( 'NONE',  ( 31.03886041246737548, -3.043338102658604161, -3.627061608673662008 ) ) ;
#10669 = CARTESIAN_POINT ( 'NONE',  ( 30.60986983071443390, -4.348964061499348333, -3.627061608673664672 ) ) ;
#10670 = EDGE_LOOP ( 'NONE', ( #4779, #652, #5462, #4566 ) ) ;
#10671 = DIRECTION ( 'NONE',  ( 1.000000000000000000, 0.000000000000000000, 0.000000000000000000 ) ) ;
#10672 = CARTESIAN_POINT ( 'NONE',  ( 2.000000000000002665, -3.464101615137751278, 0.000000000000000000 ) ) ;
#10673 = AXIS2_PLACEMENT_3D ( 'NONE', #3024, #5629, #12626 ) ;
#10674 = VERTEX_POINT ( 'NONE', #3985 ) ;
#10675 = CARTESIAN_POINT ( 'NONE',  ( 32.67202617590239555, -5.981426544730773287, 6.861505862736158257 ) ) ;
#10676 = CARTESIAN_POINT ( 'NONE',  ( 29.36638131047866906, -1.990897739957422807, -5.783357778048658915 ) ) ;
#10677 = AXIS2_PLACEMENT_3D ( 'NONE', #7435, #1639, #5961 ) ;
#10678 = LINE ( 'NONE', #13522, #12176 ) ;
#10679 = DIRECTION ( 'NONE',  ( 1.000000000000000000, 0.000000000000000000, 0.000000000000000000 ) ) ;
#10680 = CARTESIAN_POINT ( 'NONE',  ( 25.89388370423996477, -3.884438240559767497, 7.685380675815244089 ) ) ;
#10681 = CARTESIAN_POINT ( 'NONE',  ( 2.807096675499403116, -3.225959780909533503, -3.202509183706199636 ) ) ;
#10682 = CARTESIAN_POINT ( 'NONE',  ( 30.64556327217151122, -6.525384084031224496, -7.033357778048666908 ) ) ;
#10683 = ORIENTED_EDGE ( 'NONE', *, *, #9471, .T. ) ;
#10684 = CARTESIAN_POINT ( 'NONE',  ( 32.65880277236253448, -4.102108105263264193, -7.939653947423662039 ) ) ;
#10685 = CARTESIAN_POINT ( 'NONE',  ( 32.83754810739939956, -9.116730809865838836, -5.783357778048662468 ) ) ;
#10686 = LINE ( 'NONE', #17826, #3971 ) ;
#10687 = CARTESIAN_POINT ( 'NONE',  ( 4.140405595019059248, 2.228337868678515132, -3.386887224136966079 ) ) ;
#10688 = EDGE_LOOP ( 'NONE', ( #12813, #846, #13576, #7939, #7347 ) ) ;
#10689 = CARTESIAN_POINT ( 'NONE',  ( 25.95846283556873502, -3.455553161483296609, -8.283357778048658915 ) ) ;
#10690 = VECTOR ( 'NONE', #5827, 1000.000000000000000 ) ;
#10691 = EDGE_CURVE ( 'NONE', #2104, #5268, #6984, .T. ) ;
#10692 = CARTESIAN_POINT ( 'NONE',  ( 33.17547354829333983, -5.293800545841212291, -3.627061608673667781 ) ) ;
#10693 = PRESENTATION_LAYER_ASSIGNMENT (  '', '', ( #10426 ) ) ;
#10694 = ADVANCED_FACE ( 'NONE', ( #5506 ), #34, .T. ) ;
#10695 =( BOUNDED_CURVE ( )  B_SPLINE_CURVE ( 2, ( #3863, #4123, #10891, #13476, #13556, #12187, #9544, #5552, #17766 ),
 .UNSPECIFIED., .F., .T. ) 
 B_SPLINE_CURVE_WITH_KNOTS ( ( 3, 2, 2, 2, 3 ),
 ( 0.6346153846153846922, 0.6410256410256410797, 0.6538461538461538547, 0.6666666666666666297, 0.6730769230769231282 ),
 .UNSPECIFIED. ) 
 CURVE ( )  GEOMETRIC_REPRESENTATION_ITEM ( )  RATIONAL_B_SPLINE_CURVE ( ( 0.9330127018922192983, 0.9330127018922198534, 1.000000000000000000, 0.8660254037844387076, 1.000000000000000000, 0.8660254037844387076, 1.000000000000000000, 0.9330127018922187432, 0.9330127018922192983 ) ) 
 REPRESENTATION_ITEM ( '' )  );
#10696 = ORIENTED_EDGE ( 'NONE', *, *, #6293, .T. ) ;
#10697 = CARTESIAN_POINT ( 'NONE',  ( 8.874038404635943067, -3.391377654146811693, -2.000000000000000000 ) ) ;
#10698 = CARTESIAN_POINT ( 'NONE',  ( 4.000000000000000000, 2.309401076758510918, -0.5000000000000000000 ) ) ;
#10699 = ORIENTED_EDGE ( 'NONE', *, *, #4091, .T. ) ;
#10700 = CARTESIAN_POINT ( 'NONE',  ( 25.96814307759224505, -4.500799614243313762, 3.446762361689486465 ) ) ;
#10701 = DIRECTION ( 'NONE',  ( 0.000000000000000000, 0.000000000000000000, 1.000000000000000000 ) ) ;
#10702 = CARTESIAN_POINT ( 'NONE',  ( 32.93018312783485868, -2.815471066132993805, -3.627061608673662008 ) ) ;
#10703 = PRESENTATION_LAYER_ASSIGNMENT (  '', '', ( #10134 ) ) ;
#10704 = DIRECTION ( 'NONE',  ( -0.000000000000000000, -0.000000000000000000, -1.000000000000000000 ) ) ;
#10705 = ORIENTED_EDGE ( 'NONE', *, *, #7482, .F. ) ;
#10706 = CARTESIAN_POINT ( 'NONE',  ( 25.33925079868512498, -2.076342398563292058, -5.783357778048658027 ) ) ;
#10707 = DIRECTION ( 'NONE',  ( -1.000000000000000000, 0.000000000000000000, 0.000000000000000000 ) ) ;
#10708 = AXIS2_PLACEMENT_3D ( 'NONE', #4459, #9698, #24 ) ;
#10709 = FACE_OUTER_BOUND ( 'NONE', #17245, .T. ) ;
#10710 = DIRECTION ( 'NONE',  ( -0.1196152422706611984, 0.9928203230275510771, 0.000000000000000000 ) ) ;
#10711 = AXIS2_PLACEMENT_3D ( 'NONE', #9279, #5189, #10707 ) ;
#10712 = CARTESIAN_POINT ( 'NONE',  ( 26.62577407660990758, -3.575027854551694695, -3.627061608673662008 ) ) ;
#10713 = EDGE_CURVE ( 'NONE', #2135, #9702, #16270, .T. ) ;
#10714 = CARTESIAN_POINT ( 'NONE',  ( 25.93714794488954212, -2.393855775999666591, -5.783357778048658027 ) ) ;
#10715 = CARTESIAN_POINT ( 'NONE',  ( 33.20111501597313719, -6.944397359513344803, 5.783357778048657138 ) ) ;
#10716 =( GEOMETRIC_REPRESENTATION_CONTEXT ( 3 ) GLOBAL_UNCERTAINTY_ASSIGNED_CONTEXT ( ( #4085 ) ) GLOBAL_UNIT_ASSIGNED_CONTEXT ( ( #10847, #5411, #2624 ) ) REPRESENTATION_CONTEXT ( 'NONE', 'WORKASPACE' ) );
#10717 = ORIENTED_EDGE ( 'NONE', *, *, #15334, .T. ) ;
#10718 = ORIENTED_EDGE ( 'NONE', *, *, #8787, .T. ) ;
#10719 = ADVANCED_FACE ( 'NONE', ( #15218 ), #2631, .T. ) ;
#10720 = CARTESIAN_POINT ( 'NONE',  ( 30.41294626588012306, -6.253601060580800564, 4.705209693361159573 ) ) ;
#10721 = CARTESIAN_POINT ( 'NONE',  ( -17.07594129529364579, -14.18356557013591868, 15.98851070825981324 ) ) ;
#10722 = ORIENTED_EDGE ( 'NONE', *, *, #4737, .F. ) ;
#10723 = AXIS2_PLACEMENT_3D ( 'NONE', #6796, #4073, #15136 ) ;
#10724 = CARTESIAN_POINT ( 'NONE',  ( -2.100000000000000089, 2.571758278209441957E-16, -4.394516984716110741 ) ) ;
#10725 = EDGE_CURVE ( 'NONE', #13835, #2767, #10860, .T. ) ;
#10726 = CARTESIAN_POINT ( 'NONE',  ( 16.75000000000000000, -16.21813761408365195, 13.00000000000000178 ) ) ;
#10727 = CARTESIAN_POINT ( 'NONE',  ( 30.60986983071443390, -4.348964061499348333, -3.627061608673664672 ) ) ;
#10728 = CONICAL_SURFACE ( 'NONE', #15990, 2.500000000000000888, 0.9599310885968781459 ) ;
#10729 = CARTESIAN_POINT ( 'NONE',  ( 30.42903939560917337, -1.852671564043892660, -5.783357778048658027 ) ) ;
#10730 = FACE_OUTER_BOUND ( 'NONE', #6310, .T. ) ;
#10731 = SHAPE_REPRESENTATION_RELATIONSHIP ( 'NONE' , 'NONE' ,  #1480, #7249 ) ;
#10732 = CARTESIAN_POINT ( 'NONE',  ( 26.21417678486618641, -2.370676134166772808, 5.783357778048668685 ) ) ;
#10733 = EDGE_CURVE ( 'NONE', #8513, #5051, #4082, .T. ) ;
#10734 = DIRECTION ( 'NONE',  ( 0.3420201433256631063, 0.000000000000000000, 0.9396926207859104263 ) ) ;
#10735 = CARTESIAN_POINT ( 'NONE',  ( 31.24973580796908834, -6.452593224933654170, -4.533357778048668685 ) ) ;
#10736 = CARTESIAN_POINT ( 'NONE',  ( 33.46007730730551799, -5.886481946178435010, 6.861505862736157368 ) ) ;
#10737 = CIRCLE ( 'NONE', #13081, 0.2500000000000002220 ) ;
#10738 = CARTESIAN_POINT ( 'NONE',  ( 28.49145532429760053, -1.696564004353941613, 5.783357778048668685 ) ) ;
#10739 = VERTEX_POINT ( 'NONE', #2722 ) ;
#10740 = EDGE_LOOP ( 'NONE', ( #2824, #11549, #119, #8488 ) ) ;
#10741 = CIRCLE ( 'NONE', #4396, 3.999999999999998224 ) ;
#10742 = EDGE_LOOP ( 'NONE', ( #2800, #1776, #13987, #6034 ) ) ;
#10743 = CARTESIAN_POINT ( 'NONE',  ( 30.88577694472199298, -6.196634301449400084, 4.705209693361160461 ) ) ;
#10744 = DIRECTION ( 'NONE',  ( 0.000000000000000000, -0.5000000000000009992, -0.8660254037844380415 ) ) ;
#10745 = CARTESIAN_POINT ( 'NONE',  ( 30.18087924896149588, -5.654590020340094725, 7.939653947423658487 ) ) ;
#10746 = EDGE_LOOP ( 'NONE', ( #11137, #3094 ) ) ;
#10747 = CARTESIAN_POINT ( 'NONE',  ( 5.500000000000000888, -20.49999999999999645, -13.00000000000000178 ) ) ;
#10748 = CARTESIAN_POINT ( 'NONE',  ( 29.14000323013032556, -2.007974965528672495, -6.453230759126468818 ) ) ;
#10749 = EDGE_CURVE ( 'NONE', #227, #13758, #13357, .T. ) ;
#10750 = CARTESIAN_POINT ( 'NONE',  ( 27.41826274939272423, -4.733489685532582314, -8.283357778048662468 ) ) ;
#10751 = CARTESIAN_POINT ( 'NONE',  ( 29.02054416436834217, -2.659534819136519790, -4.705209693361160461 ) ) ;
#10752 = CARTESIAN_POINT ( 'NONE',  ( -15.92260893619738837, -28.39189527176317540, -12.00000000000000000 ) ) ;
#10753 = CARTESIAN_POINT ( 'NONE',  ( 32.51061761821408425, -6.300681867249914525, -4.533357778048668685 ) ) ;
#10754 = CARTESIAN_POINT ( 'NONE',  ( -29.25000000000000000, -16.21813761408365195, -13.00000000000000178 ) ) ;
#10755 = CARTESIAN_POINT ( 'NONE',  ( 26.39370705969127684, -2.976016814310973313, -6.861505862736158257 ) ) ;
#10756 = CARTESIAN_POINT ( 'NONE',  ( -45.50000000000000000, -16.03270077640482683, 8.287981825772238409 ) ) ;
#10757 = AXIS2_PLACEMENT_3D ( 'NONE', #13011, #14656, #504 ) ;
#10758 = AXIS2_PLACEMENT_3D ( 'NONE', #3977, #12490, #4064 ) ;
#10759 = CARTESIAN_POINT ( 'NONE',  ( 30.43486631442457835, -6.877930660435475296, -5.783357778048669573 ) ) ;
#10760 = ADVANCED_FACE ( 'NONE', ( #12804, #14447 ), #11430, .T. ) ;
#10761 = CARTESIAN_POINT ( 'NONE',  ( 29.54591158530375239, -2.596238420101622868, -6.861505862736158257 ) ) ;
#10762 = DIRECTION ( 'NONE',  ( 0.9928203230275512992, 0.1196152422706614898, -0.000000000000000000 ) ) ;
#10763 = CARTESIAN_POINT ( 'NONE',  ( 26.61898274975073164, -6.283600725846810953, 8.283357778048658915 ) ) ;
#10764 = ORIENTED_EDGE ( 'NONE', *, *, #8507, .F. ) ;
#10765 = EDGE_LOOP ( 'NONE', ( #15447, #17309 ) ) ;
#10766 = CARTESIAN_POINT ( 'NONE',  ( 30.88577694472199298, -6.196634301449400084, 4.705209693361160461 ) ) ;
#10767 = AXIS2_PLACEMENT_3D ( 'NONE', #6500, #12016, #14841 ) ;
#10768 = CARTESIAN_POINT ( 'NONE',  ( 27.30005507882132676, -4.747731375419166788, -3.627061608673664672 ) ) ;
#10769 = EDGE_CURVE ( 'NONE', #9967, #15002, #324, .T. ) ;
#10770 = LINE ( 'NONE', #3991, #16829 ) ;
#10771 = CARTESIAN_POINT ( 'NONE',  ( 25.71748644841968456, -2.420320648352046078, 5.783357778048663356 ) ) ;
#10772 = DIRECTION ( 'NONE',  ( 0.000000000000000000, 0.000000000000000000, -1.000000000000000000 ) ) ;
#10773 = DIRECTION ( 'NONE',  ( 0.000000000000000000, -1.000000000000000000, 1.287488025362403787E-15 ) ) ;
#10774 = CARTESIAN_POINT ( 'NONE',  ( 31.87265695910486230, -5.650636735497883478, -8.283357778048662468 ) ) ;
#10775 = ORIENTED_EDGE ( 'NONE', *, *, #7709, .F. ) ;
#10776 = VECTOR ( 'NONE', #17837, 1000.000000000000000 ) ;
#10777 = CARTESIAN_POINT ( 'NONE',  ( 33.27602027394517847, -2.146833986953896822, -4.705209693361161349 ) ) ;
#10778 = AXIS2_PLACEMENT_3D ( 'NONE', #6428, #6051, #3347 ) ;
#10779 = DIRECTION ( 'NONE',  ( 0.000000000000000000, 0.000000000000000000, 1.000000000000000000 ) ) ;
#10780 = CARTESIAN_POINT ( 'NONE',  ( 30.63309003953906995, -6.864245478665264244, -5.783357778048663356 ) ) ;
#10781 = CARTESIAN_POINT ( 'NONE',  ( 31.26353094466156080, -6.788289799823394866, 5.783357778048664244 ) ) ;
#10782 = CARTESIAN_POINT ( 'NONE',  ( 26.61898274975073164, -6.283600725846810953, -3.283357778048667797 ) ) ;
#10783 = CARTESIAN_POINT ( 'NONE',  ( 33.40754056521197413, -5.892811586081919906, -6.861505862736166250 ) ) ;
#10784 = CARTESIAN_POINT ( 'NONE',  ( 25.71748644841968456, -2.420320648352051851, -5.783357778048663356 ) ) ;
#10785 = AXIS2_PLACEMENT_3D ( 'NONE', #17800, #3891, #7887 ) ;
#10786 = ORIENTED_EDGE ( 'NONE', *, *, #13557, .F. ) ;
#10787 = DIRECTION ( 'NONE',  ( 0.1196152422706609625, -0.9928203230275510771, 0.000000000000000000 ) ) ;
#10788 = AXIS2_PLACEMENT_3D ( 'NONE', #11467, #2497, #6755 ) ;
#10789 = VERTEX_POINT ( 'NONE', #4549 ) ;
#10790 = DIRECTION ( 'NONE',  ( 0.000000000000000000, 0.000000000000000000, -1.000000000000000000 ) ) ;
#10791 = EDGE_CURVE ( 'NONE', #13499, #17849, #10342, .T. ) ;
#10792 = CARTESIAN_POINT ( 'NONE',  ( 30.18087924896149588, -5.654590020340094725, -3.627061608673668225 ) ) ;
#10793 = PLANE ( 'NONE',  #8448 ) ;
#10794 = ORIENTED_EDGE ( 'NONE', *, *, #11581, .F. ) ;
#10795 = CARTESIAN_POINT ( 'NONE',  ( 32.56242593318007295, -2.859778545457410281, -7.939653947423660263 ) ) ;
#10796 = EDGE_CURVE ( 'NONE', #17749, #11736, #15084, .T. ) ;
#10797 = FACE_BOUND ( 'NONE', #1171, .T. ) ;
#10798 = DIRECTION ( 'NONE',  ( -1.000000000000000000, -1.224646799147353454E-16, 0.000000000000000000 ) ) ;
#10799 = CARTESIAN_POINT ( 'NONE',  ( 26.37178701114681800, -2.351687214456304353, -5.783357778048658027 ) ) ;
#10800 = CARTESIAN_POINT ( 'NONE',  ( 26.31556265977298992, -7.384422263489805793, 5.783357778048663356 ) ) ;
#10801 = CARTESIAN_POINT ( 'NONE',  ( 30.37154917142620292, -2.923863409590206519, 3.283357778048666464 ) ) ;
#10802 = EDGE_LOOP ( 'NONE', ( #9943, #2585, #7250, #4088 ) ) ;
#10803 =( BOUNDED_CURVE ( )  B_SPLINE_CURVE ( 2, ( #645, #8614, #5796, #14427, #551, #4621, #12966, #14146, #6068 ),
 .UNSPECIFIED., .F., .T. ) 
 B_SPLINE_CURVE_WITH_KNOTS ( ( 3, 2, 2, 2, 3 ),
 ( 0.2884615384615384914, 0.2948717948717948789, 0.3076923076923077094, 0.3205128205128205399, 0.3269230769230769273 ),
 .UNSPECIFIED. ) 
 CURVE ( )  GEOMETRIC_REPRESENTATION_ITEM ( )  RATIONAL_B_SPLINE_CURVE ( ( 0.9330127018922194093, 0.9330127018922196314, 1.000000000000000000, 0.8660254037844387076, 1.000000000000000000, 0.8660254037844387076, 1.000000000000000000, 0.9330127018922194093, 0.9330127018922194093 ) ) 
 REPRESENTATION_ITEM ( '' )  );
#10804 = APPLICATION_CONTEXT ( 'automotive_design' ) ;
#10805 = CARTESIAN_POINT ( 'NONE',  ( 29.17398450417959310, -7.029842018119214941, 5.783357778048657138 ) ) ;
#10806 = CARTESIAN_POINT ( 'NONE',  ( -18.31874363337315970, -12.05639433133630511, 15.79760360980902689 ) ) ;
#10807 = CARTESIAN_POINT ( 'NONE',  ( -25.74999999999999645, -16.21813761408365195, 0.000000000000000000 ) ) ;
#10808 = ORIENTED_EDGE ( 'NONE', *, *, #17095, .T. ) ;
#10809 = CARTESIAN_POINT ( 'NONE',  ( 3.538288549924106796, -15.34800872113743431, -13.00000000000000178 ) ) ;
#10810 = VERTEX_POINT ( 'NONE', #10254 ) ;
#10811 = CARTESIAN_POINT ( 'NONE',  ( 38.15053902264412500, -1.114360604510109098, -1.783357778048662912 ) ) ;
#10812 = ADVANCED_FACE ( 'NONE', ( #6184 ), #5906, .F. ) ;
#10813 = ORIENTED_EDGE ( 'NONE', *, *, #7293, .T. ) ;
#10814 = LINE ( 'NONE', #7037, #2129 ) ;
#10815 = CARTESIAN_POINT ( 'NONE',  ( 29.04699097144805364, -6.418171698071525100, -4.705209693361169343 ) ) ;
#10816 = ORIENTED_EDGE ( 'NONE', *, *, #15595, .T. ) ;
#10817 = PLANE ( 'NONE',  #14454 ) ;
#10818 = CARTESIAN_POINT ( 'NONE',  ( 32.24155699611449677, -1.634298987580965923, 5.783357778048662468 ) ) ;
#10819 = DIRECTION ( 'NONE',  ( 0.9979201627913403261, -0.06446199418653550395, 5.311609029246448057E-22 ) ) ;
#10820 = CARTESIAN_POINT ( 'NONE',  ( 26.86653773853314320, -2.919050055179571945, 4.705209693361167567 ) ) ;
#10821 = EDGE_CURVE ( 'NONE', #12450, #17480, #4379, .T. ) ;
#10822 = PRODUCT_DEFINITION_SHAPE ( 'NONE', 'NONE',  #17979 ) ;
#10823 = CARTESIAN_POINT ( 'NONE',  ( 29.50659824675005893, -4.481886499472614638, 3.627061608673664228 ) ) ;
#10824 = CARTESIAN_POINT ( 'NONE',  ( -36.27615609941022257, -23.17738945083361557, -12.00000000000000000 ) ) ;
#10825 = CARTESIAN_POINT ( 'NONE',  ( 27.36943512155133362, -2.558652073080304845, -4.533357778048659803 ) ) ;
#10826 = CARTESIAN_POINT ( 'NONE',  ( 32.32618902979206865, -6.650063623909865385, 5.783357778048657138 ) ) ;
#10827 = CARTESIAN_POINT ( 'NONE',  ( 29.15568435273173264, -2.343444316361667834, 4.533357778048667797 ) ) ;
#10828 =( BOUNDED_CURVE ( )  B_SPLINE_CURVE ( 3, ( #2350, #14147, #2777, #8035 ),
 .UNSPECIFIED., .F., .T. ) 
 B_SPLINE_CURVE_WITH_KNOTS ( ( 4, 4 ),
 ( 4.715434792643774742, 4.769085813125753859 ),
 .UNSPECIFIED. ) 
 CURVE ( )  GEOMETRIC_REPRESENTATION_ITEM ( )  RATIONAL_B_SPLINE_CURVE ( ( 1.000000000000000000, 0.9997601450507493936, 0.9997601450507493936, 1.000000000000000000 ) ) 
 REPRESENTATION_ITEM ( '' )  );
#10829 = ORIENTED_EDGE ( 'NONE', *, *, #5534, .T. ) ;
#10830 = EDGE_LOOP ( 'NONE', ( #4460, #10083, #7287, #7556, #10550, #339 ) ) ;
#10831 = ORIENTED_EDGE ( 'NONE', *, *, #2225, .F. ) ;
#10832 = ORIENTED_EDGE ( 'NONE', *, *, #13233, .F. ) ;
#10833 = CARTESIAN_POINT ( 'NONE',  ( 29.99682221560115991, -1.914942061115552541, 5.783357778048668685 ) ) ;
#10834 = CARTESIAN_POINT ( 'NONE',  ( 26.01652455409633902, -4.902371455920926380, -5.783357778048663356 ) ) ;
#10835 =( REPRESENTATION_RELATIONSHIP ('NONE','NONE', #3227, #2081 ) REPRESENTATION_RELATIONSHIP_WITH_TRANSFORMATION ( #7843 )SHAPE_REPRESENTATION_RELATIONSHIP( ) );
#10836 = CARTESIAN_POINT ( 'NONE',  ( 31.45915434921569798, -2.992700983430681028, 3.627061608673666449 ) ) ;
#10837 = ORIENTED_EDGE ( 'NONE', *, *, #7392, .F. ) ;
#10838 = DIRECTION ( 'NONE',  ( 1.000000000000000000, 0.000000000000000000, 0.000000000000000000 ) ) ;
#10839 = FACE_OUTER_BOUND ( 'NONE', #10936, .T. ) ;
#10840 = DIRECTION ( 'NONE',  ( 0.000000000000000000, 0.000000000000000000, 1.000000000000000000 ) ) ;
#10841 = FACE_OUTER_BOUND ( 'NONE', #16802, .T. ) ;
#10842 = CARTESIAN_POINT ( 'NONE',  ( -9.099998387031005720, -19.29508120620799971, 6.000000000000000000 ) ) ;
#10843 = CARTESIAN_POINT ( 'NONE',  ( 0.000000000000000000, 0.000000000000000000, 6.000000000000000000 ) ) ;
#10844 = DIRECTION ( 'NONE',  ( 1.000000000000000000, 0.000000000000000000, -0.000000000000000000 ) ) ;
#10845 = CARTESIAN_POINT ( 'NONE',  ( 21.03312194624853149, -10.28219102306256971, -15.32075016948875934 ) ) ;
#10846 = CARTESIAN_POINT ( 'NONE',  ( 26.83664947211162399, -6.984282976826746037, 7.033357778048657138 ) ) ;
#10847 =( LENGTH_UNIT ( ) NAMED_UNIT ( * ) SI_UNIT ( .MILLI., .METRE. ) );
#10848 = CARTESIAN_POINT ( 'NONE',  ( 31.87075164095941915, -4.197052703815608687, -3.627061608673664672 ) ) ;
#10849 = CARTESIAN_POINT ( 'NONE',  ( 29.02054416436834217, -2.659534819136519790, -4.705209693361160461 ) ) ;
#10850 = CARTESIAN_POINT ( 'NONE',  ( -32.93004296264518160, -25.68697430340739629, 12.29384923381406658 ) ) ;
#10851 = EDGE_CURVE ( 'NONE', #12969, #17574, #3998, .T. ) ;
#10852 = CARTESIAN_POINT ( 'NONE',  ( -21.42601376483257880, 2.765314980223223529, -6.000000000000000000 ) ) ;
#10853 = ORIENTED_EDGE ( 'NONE', *, *, #13782, .F. ) ;
#10854 = CARTESIAN_POINT ( 'NONE',  ( 33.30246708102489350, -5.905470865888903020, 6.861505862736158257 ) ) ;
#10855 = CARTESIAN_POINT ( 'NONE',  ( 28.10549950023367316, -2.142809097641162897, -5.783357778048658915 ) ) ;
#10856 = DIRECTION ( 'NONE',  ( -0.000000000000000000, -0.000000000000000000, -1.000000000000000000 ) ) ;
#10857 = CARTESIAN_POINT ( 'NONE',  ( 41.90164972253716513, -2.988527579590351646, -5.783357778048662468 ) ) ;
#10858 = DIRECTION ( 'NONE',  ( 1.000000000000000000, 0.000000000000000000, 0.000000000000000000 ) ) ;
#10859 = CARTESIAN_POINT ( 'NONE',  ( 25.94006848055682468, -4.267777217026356595, 7.847536328832044994 ) ) ;
#10860 = B_SPLINE_CURVE_WITH_KNOTS ( 'NONE', 1,
 ( #5327, #1276 ),
 .UNSPECIFIED., .F., .F.,
 ( 2, 2 ),
 ( 0.000000000000000000, 1.000000000000000000 ),
 .UNSPECIFIED. ) ;
#10861 = FACE_OUTER_BOUND ( 'NONE', #5219, .T. ) ;
#10862 = CARTESIAN_POINT ( 'NONE',  ( 28.41265020943543362, -1.706058464416624787, -5.783357778048658027 ) ) ;
#10863 = ORIENTED_EDGE ( 'NONE', *, *, #4737, .T. ) ;
#10864 = CARTESIAN_POINT ( 'NONE',  ( 32.54050588463559990, -2.235448945602741766, -6.861505862736159145 ) ) ;
#10865 = CARTESIAN_POINT ( 'NONE',  ( 23.00000000000000000, -16.21813761408365195, 13.00000000000000178 ) ) ;
#10866 = CARTESIAN_POINT ( 'NONE',  ( -7.374038404635891553, 5.989453865500174778, -2.000000000000000000 ) ) ;
#10867 = FACE_OUTER_BOUND ( 'NONE', #13983, .T. ) ;
#10868 = CARTESIAN_POINT ( 'NONE',  ( 26.07857582428556853, -4.894895503279006022, -8.283357778048662468 ) ) ;
#10869 = CARTESIAN_POINT ( 'NONE',  ( 28.38593337277646711, -7.124786616671554107, -5.783357778048668685 ) ) ;
#10870 = EDGE_CURVE ( 'NONE', #11479, #15452, #14546, .T. ) ;
#10871 = LINE ( 'NONE', #8000, #17545 ) ;
#10872 = VERTEX_POINT ( 'NONE', #7385 ) ;
#10873 = CARTESIAN_POINT ( 'NONE',  ( -7.511572993685817836E-16, -4.618802153517020059, -3.133295621305386636 ) ) ;
#10874 = ORIENTED_EDGE ( 'NONE', *, *, #10457, .T. ) ;
#10875 =( LENGTH_UNIT ( ) NAMED_UNIT ( * ) SI_UNIT ( .MILLI., .METRE. ) );
#10876 = CARTESIAN_POINT ( 'NONE',  ( 31.69574812466957781, -6.726019302751734763, -5.783357778048669573 ) ) ;
#10877 = ORIENTED_EDGE ( 'NONE', *, *, #13165, .F. ) ;
#10878 = CARTESIAN_POINT ( 'NONE',  ( -5.237433445017501299, -16.51494876461869765, -16.99438405180048761 ) ) ;
#10879 = ORIENTED_EDGE ( 'NONE', *, *, #4720, .T. ) ;
#10880 = ORIENTED_EDGE ( 'NONE', *, *, #4996, .F. ) ;
#10881 = CARTESIAN_POINT ( 'NONE',  ( 32.79901970863393501, -6.593096864778464017, -5.783357778048668685 ) ) ;
#10882 = B_SPLINE_CURVE_WITH_KNOTS ( 'NONE', 3,
 ( #4299, #1590, #7123, #16823, #13095, #4561 ),
 .UNSPECIFIED., .F., .F.,
 ( 4, 2, 4 ),
 ( 0.5339563158597049330, 0.5927605480271135319, 0.6515647801945221307 ),
 .UNSPECIFIED. ) ;
#10883 = CARTESIAN_POINT ( 'NONE',  ( 0.2500000000000002220, 0.000000000000000000, 4.250000000000000000 ) ) ;
#10884 = DIRECTION ( 'NONE',  ( -0.000000000000000000, -0.000000000000000000, -1.000000000000000000 ) ) ;
#10885 = CARTESIAN_POINT ( 'NONE',  ( 26.19678349485696955, -4.880653813392439311, -3.627061608673664672 ) ) ;
#10886 = EDGE_CURVE ( 'NONE', #16703, #14159, #5469, .T. ) ;
#10887 = CARTESIAN_POINT ( 'NONE',  ( 22.62413451274595388, -22.47014588436322668, -15.00416998627796694 ) ) ;
#10888 = AXIS2_PLACEMENT_3D ( 'NONE', #10623, #16196, #11819 ) ;
#10889 = CARTESIAN_POINT ( 'NONE',  ( 30.78487334700428590, -1.819997462563214263, 5.783357778048668685 ) ) ;
#10890 = CARTESIAN_POINT ( 'NONE',  ( -16.95520570318904419, -14.57695177659950581, 16.00609026697356541 ) ) ;
#10891 = CARTESIAN_POINT ( 'NONE',  ( 28.44643833274707845, -2.428894455266221275, 4.533357778048667797 ) ) ;
#10892 = ORIENTED_EDGE ( 'NONE', *, *, #16608, .T. ) ;
#10893 = DIRECTION ( 'NONE',  ( 0.000000000000000000, 0.000000000000000000, 1.000000000000000000 ) ) ;
#10894 = DIRECTION ( 'NONE',  ( -0.9928203230275511881, -0.1196152422706606572, -1.761484381769779444E-15 ) ) ;
#10895 = ORIENTED_EDGE ( 'NONE', *, *, #968, .T. ) ;
#10896 = FACE_OUTER_BOUND ( 'NONE', #6128, .T. ) ;
#10897 = CARTESIAN_POINT ( 'NONE',  ( 31.41531425212677675, -1.744041783721344219, -5.783357778048658027 ) ) ;
#10898 = VECTOR ( 'NONE', #8260, 1000.000000000000000 ) ;
#10899 = CARTESIAN_POINT ( 'NONE',  ( 33.95908713831673964, -3.945449517755637014, 5.783357778048663356 ) ) ;
#10900 = CARTESIAN_POINT ( 'NONE',  ( 20.00000000000000000, 7.999999999999996447, 0.000000000000000000 ) ) ;
#10901 = DIRECTION ( 'NONE',  ( 1.000000000000000000, 0.000000000000000000, 0.000000000000000000 ) ) ;
#10902 = CARTESIAN_POINT ( 'NONE',  ( 29.78612525785423060, -2.267488637519798012, -7.033357778048658027 ) ) ;
#10903 =( BOUNDED_CURVE ( )  B_SPLINE_CURVE ( 3, ( #11536, #1430, #15736, #3394 ),
 .UNSPECIFIED., .F., .T. ) 
 B_SPLINE_CURVE_WITH_KNOTS ( ( 4, 4 ),
 ( 1.230954889131919305, 1.393542617697868691 ),
 .UNSPECIFIED. ) 
 CURVE ( )  GEOMETRIC_REPRESENTATION_ITEM ( )  RATIONAL_B_SPLINE_CURVE ( ( 1.000000000000000000, 0.9977983154653933262, 0.9977983154653933262, 1.000000000000000000 ) ) 
 REPRESENTATION_ITEM ( '' )  );
#10904 = CARTESIAN_POINT ( 'NONE',  ( 29.62036837594175154, -3.214238380052812261, 7.939653947423664704 ) ) ;
#10905 = AXIS2_PLACEMENT_3D ( 'NONE', #7014, #8275, #1392 ) ;
#10906 = FACE_OUTER_BOUND ( 'NONE', #17169, .T. ) ;
#10907 = CARTESIAN_POINT ( 'NONE',  ( 28.09753128235661279, -6.832371619143005503, -4.533357778048668685 ) ) ;
#10908 = CARTESIAN_POINT ( 'NONE',  ( 33.44685390376565692, -4.007163506710925027, 3.627061608673664228 ) ) ;
#10909 = ADVANCED_FACE ( 'NONE', ( #9979 ), #13078, .F. ) ;
#10910 = ORIENTED_EDGE ( 'NONE', *, *, #4835, .F. ) ;
#10911 = EDGE_LOOP ( 'NONE', ( #8877, #3793, #6025, #14457, #11378 ) ) ;
#10912 = CARTESIAN_POINT ( 'NONE',  ( 31.53813789838894621, -6.745008222462202774, 5.783357778048658027 ) ) ;
#10913 = CARTESIAN_POINT ( 'NONE',  ( 28.79925754835455010, -6.020920669644549861, -8.283357778048664244 ) ) ;
#10914 = ORIENTED_EDGE ( 'NONE', *, *, #3123, .F. ) ;
#10915 = CARTESIAN_POINT ( 'NONE',  ( 28.71854711534694715, -4.576831098024959132, 7.939653947423662039 ) ) ;
#10916 = ADVANCED_FACE ( 'NONE', ( #17087 ), #3107, .T. ) ;
#10917 = LINE ( 'NONE', #8227, #2852 ) ;
#10918 = DIRECTION ( 'NONE',  ( 0.9237280213470681067, 0.3830490080632377170, 0.000000000000000000 ) ) ;
#10919 = CARTESIAN_POINT ( 'NONE',  ( 28.63031693179632242, -2.406740715396564756, 7.033357778048666020 ) ) ;
#10920 = CIRCLE ( 'NONE', #6614, 2.749999999999995559 ) ;
#10921 = CARTESIAN_POINT ( 'NONE',  ( 25.98779870451785001, -2.387753359738024272, -6.453230759126469707 ) ) ;
#10922 = CARTESIAN_POINT ( 'NONE',  ( 28.79925754835455010, -6.020920669644549861, -8.283357778048664244 ) ) ;
#10923 = CARTESIAN_POINT ( 'NONE',  ( 29.84999239022537409, -5.894327871574777333, -3.283357778048667797 ) ) ;
#10924 = CARTESIAN_POINT ( 'NONE',  ( 8.409399735147211686E-16, 4.618802153517009401, -4.700000000000000178 ) ) ;
#10925 = CARTESIAN_POINT ( 'NONE',  ( 28.59583933521957277, -13.42685997174391765, -13.55623838816837079 ) ) ;
#10926 = CARTESIAN_POINT ( 'NONE',  ( 28.92482766011098150, -14.18604173879621477, 13.46461621778217577 ) ) ;
#10927 = ORIENTED_EDGE ( 'NONE', *, *, #12068, .T. ) ;
#10928 =( BOUNDED_CURVE ( )  B_SPLINE_CURVE ( 2, ( #16892, #1742, #12521, #7271, #11413, #16978, #11501, #10054, #15602 ),
 .UNSPECIFIED., .F., .T. ) 
 B_SPLINE_CURVE_WITH_KNOTS ( ( 3, 2, 2, 2, 3 ),
 ( 0.9038461538461538547, 0.9102564102564102422, 0.9230769230769231282, 0.9358974358974359031, 0.9423076923076922906 ),
 .UNSPECIFIED. ) 
 CURVE ( )  GEOMETRIC_REPRESENTATION_ITEM ( )  RATIONAL_B_SPLINE_CURVE ( ( 0.9330127018922194093, 0.9330127018922194093, 1.000000000000000000, 0.8660254037844387076, 1.000000000000000000, 0.8660254037844387076, 1.000000000000000000, 0.9330127018922194093, 0.9330127018922194093 ) ) 
 REPRESENTATION_ITEM ( '' )  );
#10929 = CARTESIAN_POINT ( 'NONE',  ( 31.55553118839817728, -4.235030543236534939, -7.939653947423662039 ) ) ;
#10930 = CARTESIAN_POINT ( 'NONE',  ( 27.12922144900085186, -2.887401855662130146, -4.705209693361160461 ) ) ;
#10931 = FACE_OUTER_BOUND ( 'NONE', #12707, .T. ) ;
#10932 = AXIS2_PLACEMENT_3D ( 'NONE', #9567, #13672, #4056 ) ;
#10933 = ADVANCED_FACE ( 'NONE', ( #8825 ), #1757, .T. ) ;
#10934 = CARTESIAN_POINT ( 'NONE',  ( -1.500000000000000222, -9.380831519646861238, -2.000000000000000000 ) ) ;
#10935 =( REPRESENTATION_RELATIONSHIP ('NONE','NONE', #3227, #2651 ) REPRESENTATION_RELATIONSHIP_WITH_TRANSFORMATION ( #17396 )SHAPE_REPRESENTATION_RELATIONSHIP( ) );
#10936 = EDGE_LOOP ( 'NONE', ( #12289, #7282, #11095, #11577 ) ) ;
#10937 = EDGE_LOOP ( 'NONE', ( #13943, #17147, #16707, #4017, #11778 ) ) ;
#10938 = CARTESIAN_POINT ( 'NONE',  ( 33.14902674121363901, -1.535163666906202318, 5.783357778048668685 ) ) ;
#10939 = CIRCLE ( 'NONE', #6339, 2.500000000000000888 ) ;
#10940 = CARTESIAN_POINT ( 'NONE',  ( 28.77978050244509944, -3.315512618508630549, -7.939653947423660263 ) ) ;
#10941 = DIRECTION ( 'NONE',  ( 1.000000000000000000, 0.000000000000000000, 0.000000000000000000 ) ) ;
#10942 = ORIENTED_EDGE ( 'NONE', *, *, #938, .F. ) ;
#10943 = CARTESIAN_POINT ( 'NONE',  ( 37.87429945334753256, 1.178459718517443022, -5.783357778048661579 ) ) ;
#10944 = CARTESIAN_POINT ( 'NONE',  ( 28.98992747081925359, -3.290194058894681639, -3.627061608673662896 ) ) ;
#10945 = DIRECTION ( 'NONE',  ( -1.000000000000000000, 0.000000000000000000, 0.000000000000000000 ) ) ;
#10946 = DIRECTION ( 'NONE',  ( 0.000000000000000000, 0.000000000000000000, -1.000000000000000000 ) ) ;
#10947 = CIRCLE ( 'NONE', #12418, 2.749999999999988454 ) ;
#10948 = DIRECTION ( 'NONE',  ( 0.9928203230275512992, 0.1196152422706610180, 4.006172263299093133E-17 ) ) ;
#10949 = EDGE_CURVE ( 'NONE', #12531, #1954, #3317, .T. ) ;
#10950 = CARTESIAN_POINT ( 'NONE',  ( 29.27960797773944179, -6.689954721521948144, -4.533357778048668685 ) ) ;
#10951 = ORIENTED_EDGE ( 'NONE', *, *, #11698, .T. ) ;
#10952 = DIRECTION ( 'NONE',  ( -0.000000000000000000, -0.000000000000000000, -1.000000000000000000 ) ) ;
#10953 = DIRECTION ( 'NONE',  ( 0.000000000000000000, 0.000000000000000000, 1.000000000000000000 ) ) ;
#10954 = DIRECTION ( 'NONE',  ( 0.000000000000000000, 0.000000000000000000, -1.000000000000000000 ) ) ;
#10955 = CARTESIAN_POINT ( 'NONE',  ( 31.23537658942770889, -6.791681843624433945, 6.453230759126467042 ) ) ;
#10956 = ORIENTED_EDGE ( 'NONE', *, *, #4582, .F. ) ;
#10957 = LINE ( 'NONE', #13712, #14254 ) ;
#10958 = EDGE_CURVE ( 'NONE', #10034, #13969, #14549, .T. ) ;
#10959 = CARTESIAN_POINT ( 'NONE',  ( 28.87615734162756453, -4.557842178314484016, -7.939653947423662039 ) ) ;
#10960 = AXIS2_PLACEMENT_3D ( 'NONE', #3082, #12680, #15865 ) ;
#10961 = CARTESIAN_POINT ( 'NONE',  ( 0.000000000000000000, 0.000000000000000000, 1.599999999999998979 ) ) ;
#10962 =( BOUNDED_CURVE ( )  B_SPLINE_CURVE ( 2, ( #14238, #373, #17059, #6982, #8521, #7174, #274, #5787, #10042 ),
 .UNSPECIFIED., .F., .T. ) 
 B_SPLINE_CURVE_WITH_KNOTS ( ( 3, 2, 2, 2, 3 ),
 ( 0.4423076923076923461, 0.4487179487179487336, 0.4615384615384615641, 0.4743589743589743390, 0.4807692307692307820 ),
 .UNSPECIFIED. ) 
 CURVE ( )  GEOMETRIC_REPRESENTATION_ITEM ( )  RATIONAL_B_SPLINE_CURVE ( ( 0.9330127018922194093, 0.9330127018922196314, 1.000000000000000000, 0.8660254037844387076, 1.000000000000000000, 0.8660254037844387076, 1.000000000000000000, 0.9330127018922190762, 0.9330127018922194093 ) ) 
 REPRESENTATION_ITEM ( '' )  );
#10963 = ORIENTED_EDGE ( 'NONE', *, *, #16433, .T. ) ;
#10964 = FACE_OUTER_BOUND ( 'NONE', #9527, .T. ) ;
#10965 = ORIENTED_EDGE ( 'NONE', *, *, #14376, .F. ) ;
#10966 = AXIS2_PLACEMENT_3D ( 'NONE', #12200, #1145, #2685 ) ;
#10967 = AXIS2_PLACEMENT_3D ( 'NONE', #14720, #5260, #12063 ) ;
#10968 = CARTESIAN_POINT ( 'NONE',  ( 28.89355063163679915, -2.047864499088824175, -5.783357778048658915 ) ) ;
#10969 = ADVANCED_FACE ( 'NONE', ( #12154 ), #748, .F. ) ;
#10970 = FACE_OUTER_BOUND ( 'NONE', #12624, .T. ) ;
#10971 = CIRCLE ( 'NONE', #4628, 13.00000000000000178 ) ;
#10972 = CARTESIAN_POINT ( 'NONE',  ( 26.31128205117621022, -7.047579375861630524, -7.033357778048666908 ) ) ;
#10973 = CARTESIAN_POINT ( 'NONE',  ( 25.11802603177690330, -19.03270077640482683, -10.53798182577225084 ) ) ;
#10974 = CARTESIAN_POINT ( 'NONE',  ( 32.37175601071535169, -5.590505156207296267, 8.283357778048660691 ) ) ;
#10975 = CARTESIAN_POINT ( 'NONE',  ( 27.04606801335823718, -3.524390735323772006, -7.939653947423660263 ) ) ;
#10976 = CARTESIAN_POINT ( 'NONE',  ( 29.97449477918272009, -6.943593201308171814, -5.113484796970856117 ) ) ;
#10977 = EDGE_CURVE ( 'NONE', #7401, #15874, #4618, .T. ) ;
#10978 = PRODUCT_DEFINITION ( 'UNKNOWN', '', #17901, #9158 ) ;
#10979 = AXIS2_PLACEMENT_3D ( 'NONE', #3650, #8993, #3560 ) ;
#10980 = CARTESIAN_POINT ( 'NONE',  ( 27.65911562847151117, -5.958412735707574015, 7.939653947423658487 ) ) ;
#10981 = DIRECTION ( 'NONE',  ( -0.1196152422706621005, 0.9928203230275509661, 0.000000000000000000 ) ) ;
#10982 = CARTESIAN_POINT ( 'NONE',  ( 17.60442140056922611, -19.37930158608179809, 15.90915821310915135 ) ) ;
#10983 = ORIENTED_EDGE ( 'NONE', *, *, #9120, .F. ) ;
#10984 = ORIENTED_EDGE ( 'NONE', *, *, #3088, .T. ) ;
#10985 = CARTESIAN_POINT ( 'NONE',  ( 27.42949161418789217, -3.278323244185609830, -3.283357778048662023 ) ) ;
#10986 = ADVANCED_FACE ( 'NONE', ( #5169 ), #17374, .F. ) ;
#10987 = ORIENTED_EDGE ( 'NONE', *, *, #3672, .T. ) ;
#10988 = ORIENTED_EDGE ( 'NONE', *, *, #11657, .F. ) ;
#10989 = FACE_OUTER_BOUND ( 'NONE', #1851, .T. ) ;
#10990 = AXIS2_PLACEMENT_3D ( 'NONE', #16975, #6168, #4531 ) ;
#10991 = CARTESIAN_POINT ( 'NONE',  ( 31.04338717100262102, -6.177645381738930297, -6.861505862736167138 ) ) ;
#10992 = UNCERTAINTY_MEASURE_WITH_UNIT (LENGTH_MEASURE( 1.000000000000000082E-05 ), #13485, 'distance_accuracy_value', 'NONE');
#10993 = CARTESIAN_POINT ( 'NONE',  ( -3.522881874162667515, 2.820349071481667025, -3.298443181295974469 ) ) ;
#10994 = CARTESIAN_POINT ( 'NONE',  ( 28.79241808379989465, -7.086010098929231837, -5.113484796970862334 ) ) ;
#10995 = SURFACE_SIDE_STYLE ('',( #4774 ) ) ;
#10996 = CARTESIAN_POINT ( 'NONE',  ( 32.32036211097666012, -1.624804527518282748, 5.783357778048663356 ) ) ;
#10997 = CARTESIAN_POINT ( 'NONE',  ( 27.72904566057427189, -3.442105416578422172, 7.939653947423664704 ) ) ;
#10998 = PRESENTATION_LAYER_ASSIGNMENT (  '', '', ( #17736 ) ) ;
#10999 = DIRECTION ( 'NONE',  ( 0.06446199418653537905, 0.9979201627913403261, 4.248110196704583871E-22 ) ) ;
#11000 = CARTESIAN_POINT ( 'NONE',  ( 32.43181250335191379, -6.310176327312596811, 7.033357778048657138 ) ) ;
#11001 = PLANE ( 'NONE',  #14503 ) ;
#11002 = ORIENTED_EDGE ( 'NONE', *, *, #14879, .T. ) ;
#11003 = CIRCLE ( 'NONE', #3790, 2.749999999999995559 ) ;
#11004 = EDGE_LOOP ( 'NONE', ( #16094, #5917, #11228, #4978 ) ) ;
#11005 = EDGE_LOOP ( 'NONE', ( #4456, #3620 ) ) ;
#11006 = CARTESIAN_POINT ( 'NONE',  ( 31.41114436565740320, -6.133337902414513820, 6.861505862736158257 ) ) ;
#11007 = CARTESIAN_POINT ( 'NONE',  ( 33.95908713831673964, -3.945449517755648561, 5.783357778048663356 ) ) ;
#11008 = ORIENTED_EDGE ( 'NONE', *, *, #480, .T. ) ;
#11009 = CARTESIAN_POINT ( 'NONE',  ( 30.40088504037531791, -1.856063607844930852, 5.113484796970861446 ) ) ;
#11010 = DIRECTION ( 'NONE',  ( 0.000000000000000000, 0.000000000000000000, 1.000000000000000000 ) ) ;
#11011 = DIRECTION ( 'NONE',  ( -0.1196152422706621143, 0.9928203230275509661, 0.000000000000000000 ) ) ;
#11012 = CARTESIAN_POINT ( 'NONE',  ( 33.09223089549517738, -4.049888575955752579, -8.283357778048662468 ) ) ;
#11013 = DIRECTION ( 'NONE',  ( 0.000000000000000000, 0.000000000000000000, 1.000000000000000000 ) ) ;
#11014 = CARTESIAN_POINT ( 'NONE',  ( -31.74999999999995737, 5.204748896376250699E-16, -4.250000000000000000 ) ) ;
#11015 =( BOUNDED_CURVE ( )  B_SPLINE_CURVE ( 2, ( #16455, #8277, #15446, #1395, #11069, #15257, #2836, #4381, #12630 ),
 .UNSPECIFIED., .F., .T. ) 
 B_SPLINE_CURVE_WITH_KNOTS ( ( 3, 2, 2, 2, 3 ),
 ( 0.5961538461538461453, 0.6025641025641025328, 0.6153846153846154188, 0.6282051282051281937, 0.6346153846153846922 ),
 .UNSPECIFIED. ) 
 CURVE ( )  GEOMETRIC_REPRESENTATION_ITEM ( )  RATIONAL_B_SPLINE_CURVE ( ( 0.9330127018922194093, 0.9330127018922194093, 1.000000000000000000, 0.8660254037844387076, 1.000000000000000000, 0.8660254037844387076, 1.000000000000000000, 0.9330127018922187432, 0.9330127018922192983 ) ) 
 REPRESENTATION_ITEM ( '' )  );
#11016 = VERTEX_POINT ( 'NONE', #9431 ) ;
#11018 = EDGE_CURVE ( 'NONE', #10575, #3955, #635, .T. ) ;
#11017 = CARTESIAN_POINT ( 'NONE',  ( 29.62480591732145996, -4.467644809586046151, -3.283357778048664688 ) ) ;
#11019 = CARTESIAN_POINT ( 'NONE',  ( 25.71748644841968456, -2.420320648352046078, -5.783357778048663356 ) ) ;
#11020 = DIRECTION ( 'NONE',  ( 0.000000000000000000, 0.000000000000000000, -1.000000000000000000 ) ) ;
#11021 = FACE_OUTER_BOUND ( 'NONE', #12827, .T. ) ;
#11022 = AXIS2_PLACEMENT_3D ( 'NONE', #8855, #4411, #11174 ) ;
#11023 = CARTESIAN_POINT ( 'NONE',  ( 28.91999743871649997, -5.806501378023834370, -3.627061608673668225 ) ) ;
#11024 = EDGE_CURVE ( 'NONE', #8021, #6497, #14240, .T. ) ;
#11025 = CARTESIAN_POINT ( 'NONE',  ( 28.30694982360322953, -3.372479377640031473, -7.939653947423660263 ) ) ;
#11026 = AXIS2_PLACEMENT_3D ( 'NONE', #3414, #4418, #12934 ) ;
#11027 = CARTESIAN_POINT ( 'NONE',  ( 31.92212620501791775, -6.708942077180482855, -6.453230759126470595 ) ) ;
#11028 = ORIENTED_EDGE ( 'NONE', *, *, #1484, .F. ) ;
#11029 = ORIENTED_EDGE ( 'NONE', *, *, #1420, .T. ) ;
#11030 = CARTESIAN_POINT ( 'NONE',  ( 31.41114436565740320, -6.133337902414513820, 6.861505862736158257 ) ) ;
#11031 = AXIS2_PLACEMENT_3D ( 'NONE', #250, #16486, #13761 ) ;
#11032 = CARTESIAN_POINT ( 'NONE',  ( 30.25533603959949502, -6.272589980291270351, -6.861505862736166250 ) ) ;
#11033 = CARTESIAN_POINT ( 'NONE',  ( 2.500000000000000000, 2.357898499370432166, -2.385244779468109755E-15 ) ) ;
#11034 = CARTESIAN_POINT ( 'NONE',  ( 0.000000000000000000, 0.000000000000000000, -2.000000000000000000 ) ) ;
#11035 = FACE_OUTER_BOUND ( 'NONE', #13200, .T. ) ;
#11036 = CARTESIAN_POINT ( 'NONE',  ( 27.49697864365563760, -2.843094376337701679, -6.861505862736159145 ) ) ;
#11037 = CARTESIAN_POINT ( 'NONE',  ( 0.000000000000000000, 0.000000000000000000, 13.31572692736085095 ) ) ;
#11038 = CYLINDRICAL_SURFACE ( 'NONE', #6397, 6.000000000000000888 ) ;
#11039 = VECTOR ( 'NONE', #16149, 1000.000000000000227 ) ;
#11040 = EDGE_CURVE ( 'NONE', #2553, #548, #1608, .T. ) ;
#11041 = CARTESIAN_POINT ( 'NONE',  ( 25.71748644841968456, -2.420320648352046078, -5.783357778048663356 ) ) ;
#11042 = CARTESIAN_POINT ( 'NONE',  ( 26.79905070906540132, -3.354278923027479209, -3.283357778048662023 ) ) ;
#11043 = EDGE_LOOP ( 'NONE', ( #7050, #4967, #4196, #1967 ) ) ;
#11044 = CARTESIAN_POINT ( 'NONE',  ( 31.30154412293507349, -3.011689903141150815, -7.939653947423660263 ) ) ;
#11045 = CIRCLE ( 'NONE', #367, 0.9999999999999995559 ) ;
#11046 = EDGE_CURVE ( 'NONE', #13310, #4693, #2394, .T. ) ;
#11047 = CARTESIAN_POINT ( 'NONE',  ( 28.04870365451522218, -4.657534006690712935, -8.283357778048662468 ) ) ;
#11048 = DIRECTION ( 'NONE',  ( 0.000000000000000000, -1.000000000000000000, -3.469446951953614189E-16 ) ) ;
#11049 = DIRECTION ( 'NONE',  ( -0.000000000000000000, -0.000000000000000000, 1.000000000000000000 ) ) ;
#11050 = EDGE_CURVE ( 'NONE', #6664, #11446, #2099, .T. ) ;
#11051 = CARTESIAN_POINT ( 'NONE',  ( -0.5636734750060078403, -4.293365120987107986, -3.231543764078805836 ) ) ;
#11052 = CARTESIAN_POINT ( 'NONE',  ( 30.13703915187255689, -4.405930820630744371, -7.939653947423662039 ) ) ;
#11053 = B_SPLINE_CURVE_WITH_KNOTS ( 'NONE', 3,
 ( #8968, #11680, #14417, #4789, #805, #13046, #14331, #2094, #17438, #11584, #14236, #720, #10407, #17057, #7618, #15962, #14608, #10135, #11766, #1914, #14511, #3529, #8704, #5962, #15683, #10309, #6245, #4969, #17339, #4877, #15866, #6335, #17250, #8883, #9061, #15588, #1825, #10228, #6156, #11488, #3264, #7525, #7701 ),
 .UNSPECIFIED., .F., .F.,
 ( 4, 2, 2, 1, 2, 2, 2, 2, 2, 2, 2, 2, 2, 2, 2, 2, 2, 2, 2, 2, 2, 4 ),
 ( 0.01976914256504654077, 0.02100445419277401429, 0.02162211000663775626, 0.02223976582050150169, 0.02285742163436524366, 0.02347507744822898562, 0.02471038907595646955, 0.02594570070368395695, 0.02718101233141144435, 0.02779866814527519325, 0.02841632395913894216, 0.02965163558686643996, 0.03088694721459393777, 0.03150460302845767974, 0.03212225884232142170, 0.03335757047004890563, 0.03459288209777638956, 0.03582819372550387349, 0.03644584953936762239, 0.03706350535323135742, 0.03829881698095885523, 0.03953412860868634610 ),
 .UNSPECIFIED. ) ;
#11054 = CIRCLE ( 'NONE', #3269, 3.199999999999999289 ) ;
#11055 = EDGE_CURVE ( 'NONE', #12535, #6942, #16357, .T. ) ;
#11056 = VERTEX_POINT ( 'NONE', #9175 ) ;
#11057 = CARTESIAN_POINT ( 'NONE',  ( 12.50000000000000000, 1.530808498934191521E-15, -4.000000000000000000 ) ) ;
#11058 = DIRECTION ( 'NONE',  ( -1.000000000000000000, 0.000000000000000000, 0.000000000000000000 ) ) ;
#11059 = VERTEX_POINT ( 'NONE', #3655 ) ;
#11060 = CARTESIAN_POINT ( 'NONE',  ( -16.95520570318904419, -14.57695177659950581, -16.00609026697356541 ) ) ;
#11061 = VERTEX_POINT ( 'NONE', #14719 ) ;
#11062 = CARTESIAN_POINT ( 'NONE',  ( 29.80442540930208750, -6.953886339277345563, -5.783357778048669573 ) ) ;
#11063 = DIRECTION ( 'NONE',  ( 0.000000000000000000, 0.000000000000000000, -1.000000000000000000 ) ) ;
#11064 = CIRCLE ( 'NONE', #2694, 2.500000000000001776 ) ;
#11065 = CARTESIAN_POINT ( 'NONE',  ( 25.84216048658649001, -4.923378882637265974, -3.283357778048664688 ) ) ;
#11066 = PLANE ( 'NONE',  #5120 ) ;
#11067 = CARTESIAN_POINT ( 'NONE',  ( 26.01652455409633902, -4.902371455920926380, 5.783357778048663356 ) ) ;
#11068 = CARTESIAN_POINT ( 'NONE',  ( 27.00222791626931595, -2.275731535614434531, -5.783357778048658027 ) ) ;
#11069 = CARTESIAN_POINT ( 'NONE',  ( 28.91555989733679866, -4.553094948490599592, 8.283357778048662468 ) ) ;
#11070 = AXIS2_PLACEMENT_3D ( 'NONE', #639, #15782, #14143 ) ;
#11071 = VERTEX_POINT ( 'NONE', #7994 ) ;
#11072 = EDGE_CURVE ( 'NONE', #5290, #16997, #13530, .T. ) ;
#11073 = CARTESIAN_POINT ( 'NONE',  ( 45.50000000000000000, -16.03270077640482683, -8.287981825772238409 ) ) ;
#11074 = LINE ( 'NONE', #14914, #17718 ) ;
#11075 = CARTESIAN_POINT ( 'NONE',  ( 16.95685998530892746, -17.86641812890577796, 16.00584995567978908 ) ) ;
#11076 = EDGE_LOOP ( 'NONE', ( #2421, #8302, #318, #3577, #6088, #16344, #6575, #7213, #3344, #4048, #15498 ) ) ;
#11077 = CARTESIAN_POINT ( 'NONE',  ( 30.96820195323705605, -2.125071739898741097, 4.533357778048667797 ) ) ;
#11078 = DIRECTION ( 'NONE',  ( 0.000000000000000000, 1.000000000000000000, -0.000000000000000000 ) ) ;
#11079 = CARTESIAN_POINT ( 'NONE',  ( 26.31176419598820360, -7.352894575460818594, -6.182016197336221985 ) ) ;
#11080 = CARTESIAN_POINT ( 'NONE',  ( 26.62577407660990758, -3.575027854551694695, -3.627061608673662008 ) ) ;
#11081 = ORIENTED_EDGE ( 'NONE', *, *, #15574, .F. ) ;
#11082 = CYLINDRICAL_SURFACE ( 'NONE', #12992, 5.000000000000000000 ) ;
#11083 = CARTESIAN_POINT ( 'NONE',  ( 28.58911057998038885, -6.046239229258517867, -3.283357778048667797 ) ) ;
#11084 = CARTESIAN_POINT ( 'NONE',  ( -10.27627944162886209, -4.200961894323246071, -3.000000000000000888 ) ) ;
#11085 = CARTESIAN_POINT ( 'NONE',  ( 28.76238721243587193, -5.825490297734302381, 7.939653947423658487 ) ) ;
#11086 = CARTESIAN_POINT ( 'NONE',  ( 28.11132641904908169, -7.168068194032743534, -5.783357778048668685 ) ) ;
#11087 = CARTESIAN_POINT ( 'NONE',  ( 13.00000000000000178, 0.000000000000000000, -12.00000000000000000 ) ) ;
#11088 = CARTESIAN_POINT ( 'NONE',  ( 32.04575515724926760, -1.668086104879473730, 5.783357778048668685 ) ) ;
#11089 = EDGE_CURVE ( 'NONE', #2542, #11393, #6467, .T. ) ;
#11090 = ORIENTED_EDGE ( 'NONE', *, *, #16397, .F. ) ;
#11091 = EDGE_CURVE ( 'NONE', #2761, #1161, #12088, .T. ) ;
#11092 = ORIENTED_EDGE ( 'NONE', *, *, #17947, .T. ) ;
#11093 = CARTESIAN_POINT ( 'NONE',  ( 27.08121146544255353, -6.028038774645947839, 3.627061608673662896 ) ) ;
#11094 = CARTESIAN_POINT ( 'NONE',  ( -45.00000000000000711, -19.03270077640482683, 10.53798182577225084 ) ) ;
#11095 = ORIENTED_EDGE ( 'NONE', *, *, #3542, .T. ) ;
#11096 = CARTESIAN_POINT ( 'NONE',  ( 27.75966235412334981, -2.811446176820259879, 6.861505862736166250 ) ) ;
#11097 = EDGE_LOOP ( 'NONE', ( #13386, #2659, #5030, #11352 ) ) ;
#11098 = DIRECTION ( 'NONE',  ( -0.1196152422706610735, 0.9928203230275511881, 0.000000000000000000 ) ) ;
#11099 = CARTESIAN_POINT ( 'NONE',  ( -45.50000000000000000, -19.03270077640483038, 8.287981825772241962 ) ) ;
#11100 = FACE_OUTER_BOUND ( 'NONE', #7515, .T. ) ;
#11101 = CARTESIAN_POINT ( 'NONE',  ( 26.63030083514515312, -6.709335133632020387, -6.861505862736167138 ) ) ;
#11102 = CARTESIAN_POINT ( 'NONE',  ( 26.31556265977298992, -7.384422263489805793, -5.783357778048663356 ) ) ;
#11103 = CARTESIAN_POINT ( 'NONE',  ( 28.79925754835455010, -6.020920669644549861, -8.283357778048662468 ) ) ;
#11104 = CARTESIAN_POINT ( 'NONE',  ( 45.50000000000000000, -16.03270077640482683, -5.537981825772250843 ) ) ;
#11105 = CARTESIAN_POINT ( 'NONE',  ( 16.91330062320331962, -14.78391025039656625, -16.01216328675237577 ) ) ;
#11106 = CARTESIAN_POINT ( 'NONE',  ( 28.29479612530171551, -12.89112598890823946, 13.63906826012424922 ) ) ;
#11107 = CARTESIAN_POINT ( 'NONE',  ( 29.38830135902312080, -2.615227339812091767, -6.861505862736159145 ) ) ;
#11108 = CARTESIAN_POINT ( 'NONE',  ( 28.41655006632555569, -6.494127376913395366, -4.705209693361169343 ) ) ;
#11109 = EDGE_LOOP ( 'NONE', ( #8526, #7645 ) ) ;
#11110 = DIRECTION ( 'NONE',  ( -1.000000000000000000, 0.000000000000000000, 0.000000000000000000 ) ) ;
#11111 = VERTEX_POINT ( 'NONE', #7091 ) ;
#11112 = ADVANCED_FACE ( 'NONE', ( #5698 ), #11215, .F. ) ;
#11113 = ORIENTED_EDGE ( 'NONE', *, *, #501, .F. ) ;
#11114 = CARTESIAN_POINT ( 'NONE',  ( 27.62849893492243325, -6.589071975465733644, 6.861505862736158257 ) ) ;
#11115 = CARTESIAN_POINT ( 'NONE',  ( 26.49461065740898391, -7.352653653197164907, -5.783357778048668685 ) ) ;
#11116 = DIRECTION ( 'NONE',  ( 0.9928203230275514102, 0.1196152422706598939, 0.000000000000000000 ) ) ;
#11117 = CARTESIAN_POINT ( 'NONE',  ( 25.76974524478944062, -2.854074692636065169, -5.141149657938114181 ) ) ;
#11118 = CARTESIAN_POINT ( 'NONE',  ( 30.05650519998692971, -5.408673599982567026, -13.28483438372752445 ) ) ;
#11119 = CARTESIAN_POINT ( 'NONE',  ( 30.12381574833269937, -2.526612381163247267, -4.705209693361161349 ) ) ;
#11120 = CARTESIAN_POINT ( 'NONE',  ( 31.51612863268893960, -4.239777773060436239, -3.283357778048664688 ) ) ;
#11121 = EDGE_CURVE ( 'NONE', #254, #16114, #10737, .T. ) ;
#11122 = LINE ( 'NONE', #5693, #13639 ) ;
#11123 = MANIFOLD_SOLID_BREP ( 'Cavity1', #10432 ) ;
#11124 = CARTESIAN_POINT ( 'NONE',  ( 35.74085044863416982, -23.57886868891565513, -11.27079897466147251 ) ) ;
#11125 = CARTESIAN_POINT ( 'NONE',  ( 27.33945763453056088, -4.742984145595265488, -8.283357778048662468 ) ) ;
#11126 = CARTESIAN_POINT ( 'NONE',  ( 29.36638131047866196, -1.990897739957422807, -5.783357778048658027 ) ) ;
#11127 = AXIS2_PLACEMENT_3D ( 'NONE', #13823, #3873, #4038 ) ;
#11128 =( NAMED_UNIT ( * ) PLANE_ANGLE_UNIT ( ) SI_UNIT ( $, .RADIAN. ) );
#11129 = FACE_OUTER_BOUND ( 'NONE', #12308, .T. ) ;
#11130 = CARTESIAN_POINT ( 'NONE',  ( 31.26353094466156080, -6.788289799823394866, -5.783357778048663356 ) ) ;
#11131 = CARTESIAN_POINT ( 'NONE',  ( 32.82573654529290508, -1.174368712523534475, 5.783357778048668685 ) ) ;
#11132 = CARTESIAN_POINT ( 'NONE',  ( 28.73594040535617467, -2.066853418799292630, -5.783357778048658915 ) ) ;
#11133 = ADVANCED_FACE ( 'NONE', ( #4003 ), #8442, .T. ) ;
#11134 = VERTEX_POINT ( 'NONE', #1200 ) ;
#11135 = CARTESIAN_POINT ( 'NONE',  ( 32.36819060393585801, 0.8990368551114588103, -5.783357778048663356 ) ) ;
#11136 = CARTESIAN_POINT ( 'NONE',  ( 0.000000000000000000, 0.000000000000000000, -2.000000000000000000 ) ) ;
#11137 = ORIENTED_EDGE ( 'NONE', *, *, #17392, .T. ) ;
#11138 = LINE ( 'NONE', #1571, #3534 ) ;
#11139 = ORIENTED_EDGE ( 'NONE', *, *, #5413, .T. ) ;
#11140 = ADVANCED_FACE ( 'NONE', ( #9516 ), #4271, .F. ) ;
#11141 = CARTESIAN_POINT ( 'NONE',  ( 31.45915434921569798, -2.992700983430681028, -7.939653947423660263 ) ) ;
#11142 = DIRECTION ( 'NONE',  ( -0.000000000000000000, 1.000000000000000000, 0.000000000000000000 ) ) ;
#11143 = ORIENTED_EDGE ( 'NONE', *, *, #335, .T. ) ;
#11144 = CARTESIAN_POINT ( 'NONE',  ( 31.51169109130924184, -2.986371343527201905, -3.627061608673662896 ) ) ;
#11145 = DIRECTION ( 'NONE',  ( 0.000000000000000000, 0.000000000000000000, 1.000000000000000000 ) ) ;
#11146 = DIRECTION ( 'NONE',  ( -0.9985081203071058953, 0.05460342187784718998, -9.468742811518590322E-17 ) ) ;
#11147 = VERTEX_POINT ( 'NONE', #1290 ) ;
#11148 = CARTESIAN_POINT ( 'NONE',  ( 30.33776104811456165, -2.201027418740610919, -7.033357778048658027 ) ) ;
#11149 = CARTESIAN_POINT ( 'NONE',  ( 19.91592223102268733, -21.66952118561269458, -15.52717098632164117 ) ) ;
#11150 = EDGE_LOOP ( 'NONE', ( #7010, #14200, #14131, #11653 ) ) ;
#11151 = CARTESIAN_POINT ( 'NONE',  ( 30.06013935859953534, -5.869009311960810216, 3.283357778048663800 ) ) ;
#11152 = CARTESIAN_POINT ( 'NONE',  ( 26.52522735095806894, -6.721994413439005278, 6.861505862736157368 ) ) ;
#11153 = FILL_AREA_STYLE ('',( #12633 ) ) ;
#11154 = CARTESIAN_POINT ( 'NONE',  ( -35.74085044863416272, -18.73429073671335132, 11.27079897466147607 ) ) ;
#11155 = ORIENTED_EDGE ( 'NONE', *, *, #6483, .T. ) ;
#11156 = CARTESIAN_POINT ( 'NONE',  ( 32.34167700165585302, -2.686501913001913433, -8.283357778048660691 ) ) ;
#11157 = ORIENTED_EDGE ( 'NONE', *, *, #9820, .T. ) ;
#11158 = FACE_OUTER_BOUND ( 'NONE', #13644, .T. ) ;
#11159 = ORIENTED_EDGE ( 'NONE', *, *, #16525, .T. ) ;
#11160 = CARTESIAN_POINT ( 'NONE',  ( 39.55500000000002103, 0.000000000000000000, 2.500000000000000888 ) ) ;
#11161 = CARTESIAN_POINT ( 'NONE',  ( 25.78518620311324838, -3.676302093007511651, -7.939653947423660263 ) ) ;
#11162 = EDGE_CURVE ( 'NONE', #15456, #14684, #6814, .T. ) ;
#11163 = CARTESIAN_POINT ( 'NONE',  ( 31.15208055228630357, -2.102918000029084578, -4.533357778048659803 ) ) ;
#11164 = DIRECTION ( 'NONE',  ( 0.000000000000000000, 1.000000000000000000, -1.103561164596346103E-15 ) ) ;
#11165 =( NAMED_UNIT ( * ) PLANE_ANGLE_UNIT ( ) SI_UNIT ( $, .RADIAN. ) );
#11166 = CARTESIAN_POINT ( 'NONE',  ( 0.000000000000000000, 0.000000000000000000, -1.901951201008075243 ) ) ;
#11167 = CARTESIAN_POINT ( 'NONE',  ( 28.98992747081925359, -3.290194058894681639, 7.939653947423664704 ) ) ;
#11168 = DIRECTION ( 'NONE',  ( 0.9928203230275512992, 0.1196152422706610180, 4.006172263299093133E-17 ) ) ;
#11169 = CARTESIAN_POINT ( 'NONE',  ( -36.95907006869318678, -17.52584492564777818, 5.783357778048664244 ) ) ;
#11170 = CARTESIAN_POINT ( 'NONE',  ( 31.02146712245815507, -5.553315781884258229, 3.627061608673662896 ) ) ;
#11171 = VERTEX_POINT ( 'NONE', #9 ) ;
#11172 = VERTEX_POINT ( 'NONE', #9600 ) ;
#11173 = CARTESIAN_POINT ( 'NONE',  ( 30.15026255541241440, -6.285249260098253465, 6.861505862736158257 ) ) ;
#11174 = DIRECTION ( 'NONE',  ( -0.1196152422706611984, 0.9928203230275510771, 0.000000000000000000 ) ) ;
#11175 = CARTESIAN_POINT ( 'NONE',  ( 0.000000000000000000, 0.000000000000000000, -2.000000000000000000 ) ) ;
#11176 = VERTEX_POINT ( 'NONE', #1371 ) ;
#11177 = CARTESIAN_POINT ( 'NONE',  ( 27.86926259684567597, -5.933094176093607786, 3.627061608673662896 ) ) ;
#11178 = AXIS2_PLACEMENT_3D ( 'NONE', #12424, #2904, #11312 ) ;
#11179 = PRODUCT_DEFINITION_FORMATION_WITH_SPECIFIED_SOURCE ( 'ANY', '', #13304, .NOT_KNOWN. ) ;
#11180 = CARTESIAN_POINT ( 'NONE',  ( -23.00000000000000000, -16.21813761408365195, 13.00000000000000178 ) ) ;
#11181 = DIRECTION ( 'NONE',  ( 0.9928203230275512992, 0.1196152422706610180, 4.006172263299093133E-17 ) ) ;
#11182 = DIRECTION ( 'NONE',  ( 1.000000000000000000, 0.000000000000000000, 0.000000000000000000 ) ) ;
#11183 = CARTESIAN_POINT ( 'NONE',  ( 27.65911562847151117, -5.958412735707574015, -3.627061608673668225 ) ) ;
#11184 = DIRECTION ( 'NONE',  ( 0.000000000000000000, 0.000000000000000000, 1.000000000000000000 ) ) ;
#11185 = CARTESIAN_POINT ( 'NONE',  ( 30.45035428628836627, -2.914368949527523789, -8.283357778048658915 ) ) ;
#11186 = VECTOR ( 'NONE', #12901, 999.9999999999998863 ) ;
#11187 = EDGE_CURVE ( 'NONE', #6885, #15376, #8435, .T. ) ;
#11188 = DIRECTION ( 'NONE',  ( 1.000000000000000000, 0.000000000000000000, 0.000000000000000000 ) ) ;
#11189 = DIRECTION ( 'NONE',  ( -1.000000000000000000, 0.000000000000000000, -0.000000000000000000 ) ) ;
#11190 = SURFACE_SIDE_STYLE ('',( #11570 ) ) ;
#11191 = CARTESIAN_POINT ( 'NONE',  ( 32.75517961154501023, -5.344437665069116328, -7.939653947423664704 ) ) ;
#11192 = ORIENTED_EDGE ( 'NONE', *, *, #8507, .T. ) ;
#11193 = DIRECTION ( 'NONE',  ( 0.000000000000000000, 1.000000000000000000, 0.000000000000000000 ) ) ;
#11194 = DIRECTION ( 'NONE',  ( -0.1196152422706611151, 0.9928203230275511881, 0.000000000000000000 ) ) ;
#11195 = ADVANCED_FACE ( 'NONE', ( #9773 ), #1793, .T. ) ;
#11196 = ORIENTED_EDGE ( 'NONE', *, *, #13061, .F. ) ;
#11197 = ORIENTED_EDGE ( 'NONE', *, *, #5958, .T. ) ;
#11198 = PRESENTATION_LAYER_ASSIGNMENT (  '', '', ( #8047 ) ) ;
#11199 = ORIENTED_EDGE ( 'NONE', *, *, #9926, .T. ) ;
#11200 = CARTESIAN_POINT ( 'NONE',  ( 28.35948656569676629, -3.366149737736551906, 7.939653947423662927 ) ) ;
#11201 = CARTESIAN_POINT ( 'NONE',  ( 28.91555989733679866, -4.553094948490599592, -3.283357778048664688 ) ) ;
#11202 = CARTESIAN_POINT ( 'NONE',  ( -2.500000000000000888, 3.061616997868384127E-16, -4.699999999999999289 ) ) ;
#11203 = CARTESIAN_POINT ( 'NONE',  ( 13.00000000000000178, 0.000000000000000000, 12.00000000000000000 ) ) ;
#11204 = CARTESIAN_POINT ( 'NONE',  ( 26.01652455409633902, -4.902371455920926380, 5.783357778048663356 ) ) ;
#11205 = CARTESIAN_POINT ( 'NONE',  ( 29.62489513447700062, -6.348545659133139729, -6.861505862736166250 ) ) ;
#11206 = CARTESIAN_POINT ( 'NONE',  ( -36.07773319708005744, -23.32620662758124297, -11.14818368178938357 ) ) ;
#11207 = CARTESIAN_POINT ( 'NONE',  ( 0.000000000000000000, 0.000000000000000000, -12.00000000000000000 ) ) ;
#11208 = CARTESIAN_POINT ( 'NONE',  ( 45.00000000000000711, -19.03270077640482683, -10.53798182577225084 ) ) ;
#11209 = EDGE_CURVE ( 'NONE', #11560, #2108, #17457, .T. ) ;
#11210 = CARTESIAN_POINT ( 'NONE',  ( 27.96989853965305528, -4.667028466753395222, -8.283357778048662468 ) ) ;
#11211 = AXIS2_PLACEMENT_3D ( 'NONE', #10899, #9383, #4221 ) ;
#11212 = ORIENTED_EDGE ( 'NONE', *, *, #201, .T. ) ;
#11213 = CARTESIAN_POINT ( 'NONE',  ( 30.01874226414561875, -2.539271660970221944, -6.861505862736159145 ) ) ;
#11214 = VECTOR ( 'NONE', #16474, 1000.000000000000114 ) ;
#11215 = CYLINDRICAL_SURFACE ( 'NONE', #16864, 6.249999999999998224 ) ;
#11216 = DIRECTION ( 'NONE',  ( 0.000000000000000000, 0.000000000000000000, -1.000000000000000000 ) ) ;
#11217 = CARTESIAN_POINT ( 'NONE',  ( 4.211140560182196957, -2.431303136016550237, -3.445885042887436800 ) ) ;
#11218 = FACE_OUTER_BOUND ( 'NONE', #8264, .T. ) ;
#11219 = CARTESIAN_POINT ( 'NONE',  ( 32.22908376348204484, -1.973160382215000785, 4.533357778048667797 ) ) ;
#11220 = CARTESIAN_POINT ( 'NONE',  ( 29.82181869931131146, -4.443908660051686610, -3.627061608673664672 ) ) ;
#11221 = EDGE_LOOP ( 'NONE', ( #6702, #15971, #2759, #6746 ) ) ;
#11222 = VERTEX_POINT ( 'NONE', #5754 ) ;
#11223 = FACE_OUTER_BOUND ( 'NONE', #10398, .T. ) ;
#11224 = FACE_OUTER_BOUND ( 'NONE', #7946, .T. ) ;
#11225 = CIRCLE ( 'NONE', #2576, 2.749999999999988454 ) ;
#11226 = ORIENTED_EDGE ( 'NONE', *, *, #13488, .F. ) ;
#11227 = DIRECTION ( 'NONE',  ( 0.000000000000000000, 0.000000000000000000, -1.000000000000000000 ) ) ;
#11228 = ORIENTED_EDGE ( 'NONE', *, *, #9165, .T. ) ;
#11229 = CARTESIAN_POINT ( 'NONE',  ( 29.25000000000000000, -16.21813761408365195, 13.00000000000000178 ) ) ;
#11230 = AXIS2_PLACEMENT_3D ( 'NONE', #13009, #12917, #857 ) ;
#11231 = ORIENTED_EDGE ( 'NONE', *, *, #16302, .T. ) ;
#11232 = EDGE_CURVE ( 'NONE', #17258, #9429, #13951, .T. ) ;
#11233 = ORIENTED_EDGE ( 'NONE', *, *, #17416, .T. ) ;
#11234 = CARTESIAN_POINT ( 'NONE',  ( 28.73594040535616756, -2.066853418799292630, -5.783357778048658027 ) ) ;
#11235 = DIRECTION ( 'NONE',  ( 0.000000000000000000, 0.000000000000000000, 1.000000000000000000 ) ) ;
#11236 = CARTESIAN_POINT ( 'NONE',  ( 4.000000000000000000, -1.700153365595038268, -3.020323189000620800 ) ) ;
#11237 = ORIENTED_EDGE ( 'NONE', *, *, #7326, .F. ) ;
#11238 = CARTESIAN_POINT ( 'NONE',  ( 32.29295089585319545, -5.599999616269980329, -3.283357778048667797 ) ) ;
#11239 = AXIS2_PLACEMENT_3D ( 'NONE', #9259, #17824, #2737 ) ;
#11240 = CARTESIAN_POINT ( 'NONE',  ( 31.59864285835955400, -2.049116061056871274, -7.033357778048658027 ) ) ;
#11241 = CARTESIAN_POINT ( 'NONE',  ( 33.60446413004628141, -3.988174587000466342, 7.939653947423662039 ) ) ;
#11242 = VECTOR ( 'NONE', #11841, 1000.000000000000000 ) ;
#11243 = CARTESIAN_POINT ( 'NONE',  ( 27.65458886993626564, -2.824105456627233224, 4.705209693361168455 ) ) ;
#11244 = CARTESIAN_POINT ( 'NONE',  ( 33.21234388421201800, -5.489230917751459771, 3.283357778048663356 ) ) ;
#11245 = ORIENTED_EDGE ( 'NONE', *, *, #14215, .F. ) ;
#11246 = CARTESIAN_POINT ( 'NONE',  ( 32.32036211097666012, -1.624804527518282748, -5.783357778048663356 ) ) ;
#11247 = EDGE_LOOP ( 'NONE', ( #6150, #3964, #15086, #8939, #7568 ) ) ;
#11248 = AXIS2_PLACEMENT_3D ( 'NONE', #7256, #8797, #10308 ) ;
#11249 = CARTESIAN_POINT ( 'NONE',  ( 7.958171371211042455, 6.326703190994719783, -2.666481567098319960 ) ) ;
#11250 = ORIENTED_EDGE ( 'NONE', *, *, #14893, .T. ) ;
#11251 = LINE ( 'NONE', #12914, #12806 ) ;
#11252 = CARTESIAN_POINT ( 'NONE',  ( 25.74134610602432360, -2.427642893298174620, -5.783357778048658027 ) ) ;
#11253 = EDGE_CURVE ( 'NONE', #6928, #13340, #11304, .T. ) ;
#11254 = CARTESIAN_POINT ( 'NONE',  ( 32.37175601071535880, -5.590505156207296267, -3.283357778048667797 ) ) ;
#11255 = DIRECTION ( 'NONE',  ( 0.9928203230275512992, 0.1196152422706610180, 4.006172263299093133E-17 ) ) ;
#11256 = APPLICATION_PROTOCOL_DEFINITION ( 'draft international standard', 'automotive_design', 1998, #11649 ) ;
#11257 = DIRECTION ( 'NONE',  ( 0.000000000000000000, 0.000000000000000000, -1.000000000000000000 ) ) ;
#11258 = CARTESIAN_POINT ( 'NONE',  ( 33.13163345120441505, -4.045141346131868154, -3.627061608673664672 ) ) ;
#11259 = FACE_OUTER_BOUND ( 'NONE', #15717, .T. ) ;
#11260 = CARTESIAN_POINT ( 'NONE',  ( 31.61111609099199171, -1.710254666422835745, 5.783357778048665132 ) ) ;
#11261 = EDGE_CURVE ( 'NONE', #5316, #14093, #7143, .T. ) ;
#11262 = CARTESIAN_POINT ( 'NONE',  ( 31.44176105920648823, -5.502678662656354192, 7.939653947423658487 ) ) ;
#11263 = AXIS2_PLACEMENT_3D ( 'NONE', #5760, #12933, #347 ) ;
#11264 = EDGE_LOOP ( 'NONE', ( #7962, #12582, #9547, #9145 ) ) ;
#11265 = ORIENTED_EDGE ( 'NONE', *, *, #603, .T. ) ;
#11266 = EDGE_CURVE ( 'NONE', #14073, #6202, #4320, .T. ) ;
#11267 = CARTESIAN_POINT ( 'NONE',  ( 29.82181869931131146, -4.443908660051686610, 7.939653947423662039 ) ) ;
#11268 = DIRECTION ( 'NONE',  ( 0.9928203230275510771, 0.1196152422706614621, -0.000000000000000000 ) ) ;
#11269 = CARTESIAN_POINT ( 'NONE',  ( 26.27749392786456895, -6.324743385012030927, -8.283357778048664244 ) ) ;
#11270 = VECTOR ( 'NONE', #3747, 1000.000000000000000 ) ;
#11271 = VERTEX_POINT ( 'NONE', #7416 ) ;
#11272 = CARTESIAN_POINT ( 'NONE',  ( 26.49878054387835746, -2.963357534503999968, 6.861505862736166250 ) ) ;
#11273 =( BOUNDED_CURVE ( )  B_SPLINE_CURVE ( 2, ( #2783, #13581, #13755, #15021, #12307, #10913, #1163, #16659, #6682 ),
 .UNSPECIFIED., .F., .T. ) 
 B_SPLINE_CURVE_WITH_KNOTS ( ( 3, 2, 2, 2, 3 ),
 ( 0.5576923076923077094, 0.5641025641025640969, 0.5769230769230768718, 0.5897435897435897578, 0.5961538461538461453 ),
 .UNSPECIFIED. ) 
 CURVE ( )  GEOMETRIC_REPRESENTATION_ITEM ( )  RATIONAL_B_SPLINE_CURVE ( ( 0.9330127018922194093, 0.9330127018922194093, 1.000000000000000000, 0.8660254037844387076, 1.000000000000000000, 0.8660254037844387076, 1.000000000000000000, 0.9330127018922194093, 0.9330127018922194093 ) ) 
 REPRESENTATION_ITEM ( '' )  );
#11274 = CYLINDRICAL_SURFACE ( 'NONE', #15890, 2.500000000000001776 ) ;
#11275 = CARTESIAN_POINT ( 'NONE',  ( 0.000000000000000000, 0.000000000000000000, -3.700000000000000178 ) ) ;
#11276 = CARTESIAN_POINT ( 'NONE',  ( 0.000000000000000000, 0.000000000000000000, -10.00000000000000000 ) ) ;
#11277 = CARTESIAN_POINT ( 'NONE',  ( 30.63309003953906995, -6.864245478665264244, -5.783357778048663356 ) ) ;
#11278 =( REPRESENTATION_RELATIONSHIP ('NONE','NONE', #3227, #2081 ) REPRESENTATION_RELATIONSHIP_WITH_TRANSFORMATION ( #11817 )SHAPE_REPRESENTATION_RELATIONSHIP( ) );
#11279 = CARTESIAN_POINT ( 'NONE',  ( 27.02423718196931546, -4.780961985016209503, -3.283357778048664688 ) ) ;
#11280 = CARTESIAN_POINT ( 'NONE',  ( 30.75815651034531584, -7.238725614818142695, -5.783357778048669573 ) ) ;
#11281 = COLOUR_RGB ( '', 0.31764706, 0.68627451, 0.89019608) ;
#11282 = DIRECTION ( 'NONE',  ( 0.000000000000000000, 0.000000000000000000, 1.000000000000000000 ) ) ;
#11283 = DIRECTION ( 'NONE',  ( -1.000000000000000000, 0.000000000000000000, 0.000000000000000000 ) ) ;
#11284 = FILL_AREA_STYLE_COLOUR ( '', #617 ) ;
#11285 = CARTESIAN_POINT ( 'NONE',  ( 32.64557936882268052, -2.222789665795767089, -4.705209693361161349 ) ) ;
#11286 = VERTEX_POINT ( 'NONE', #14306 ) ;
#11287 = CARTESIAN_POINT ( 'NONE',  ( 26.49878054387835746, -2.963357534503999968, -4.705209693361160461 ) ) ;
#11288 = AXIS2_PLACEMENT_3D ( 'NONE', #8636, #4642, #14166 ) ;
#11289 = CARTESIAN_POINT ( 'NONE',  ( 27.48088551392658729, -7.244023872874614689, -5.783357778048657138 ) ) ;
#11290 = EDGE_LOOP ( 'NONE', ( #7476, #17509, #13360, #14481, #3233, #15733 ) ) ;
#11291 = ORIENTED_EDGE ( 'NONE', *, *, #17759, .T. ) ;
#11292 = ORIENTED_EDGE ( 'NONE', *, *, #9234, .F. ) ;
#11293 = EDGE_CURVE ( 'NONE', #13537, #8906, #10170, .T. ) ;
#11294 = CARTESIAN_POINT ( 'NONE',  ( 28.56093688906631911, -4.595820017735426255, 7.939653947423662039 ) ) ;
#11295 = EDGE_LOOP ( 'NONE', ( #5559, #6451, #3103, #9751 ) ) ;
#11296 = CARTESIAN_POINT ( 'NONE',  ( 26.23609683341064525, -2.995005734021441768, -6.861505862736159145 ) ) ;
#11297 = CARTESIAN_POINT ( 'NONE',  ( 32.96626681528915981, -4.065064760026301016, -5.783357778048663356 ) ) ;
#11298 = PLANE ( 'NONE',  #3755 ) ;
#11299 = CARTESIAN_POINT ( 'NONE',  ( 28.99436501219896201, -4.543600488427916417, -3.283357778048664688 ) ) ;
#11301 = CIRCLE ( 'NONE', #13643, 9.500000000000000000 ) ;
#11300 = CARTESIAN_POINT ( 'NONE',  ( 32.07220196432897552, -5.426722983814484813, -3.627061608673668225 ) ) ;
#11302 = LINE ( 'NONE', #15504, #1787 ) ;
#11303 = LINE ( 'NONE', #3533, #13917 ) ;
#11304 = CIRCLE ( 'NONE', #2941, 0.5155456020628804703 ) ;
#11305 = DIRECTION ( 'NONE',  ( 1.000000000000000000, 0.000000000000000000, 0.000000000000000000 ) ) ;
#11306 = EDGE_CURVE ( 'NONE', #6149, #10652, #17705, .T. ) ;
#11307 = CARTESIAN_POINT ( 'NONE',  ( 26.24565837299761739, -7.163851760794091916, -7.234565377303040279 ) ) ;
#11308 = VECTOR ( 'NONE', #7988, 1000.000000000000227 ) ;
#11309 = VERTEX_POINT ( 'NONE', #14112 ) ;
#11310 = CARTESIAN_POINT ( 'NONE',  ( 29.62489513447700062, -6.348545659133139729, -6.861505862736166250 ) ) ;
#11311 = PLANE ( 'NONE',  #1470 ) ;
#11312 = DIRECTION ( 'NONE',  ( -0.1196152422706611984, 0.9928203230275510771, 0.000000000000000000 ) ) ;
#11313 = CARTESIAN_POINT ( 'NONE',  ( 2.100000000000000089, 0.000000000000000000, -4.700000000000000178 ) ) ;
#11314 = ORIENTED_EDGE ( 'NONE', *, *, #15032, .F. ) ;
#11315 = CARTESIAN_POINT ( 'NONE',  ( 29.32081432955537892, -3.050456207659999475, 8.283357778048664244 ) ) ;
#11316 = CARTESIAN_POINT ( 'NONE',  ( 26.87106449706838873, -6.053357334259913181, -3.627061608673667781 ) ) ;
#11317 = AXIS2_PLACEMENT_3D ( 'NONE', #946, #17576, #5096 ) ;
#11318 = AXIS2_PLACEMENT_3D ( 'NONE', #9183, #10265, #16097 ) ;
#11319 = ORIENTED_EDGE ( 'NONE', *, *, #8350, .T. ) ;
#11320 = ORIENTED_EDGE ( 'NONE', *, *, #2690, .F. ) ;
#11321 = ADVANCED_FACE ( 'NONE', ( #15655 ), #8738, .T. ) ;
#11322 = ORIENTED_EDGE ( 'NONE', *, *, #1459, .T. ) ;
#11323 = LINE ( 'NONE', #3186, #17214 ) ;
#11324 = CIRCLE ( 'NONE', #5594, 2.041999999999999815 ) ;
#11325 = VECTOR ( 'NONE', #3002, 1000.000000000000000 ) ;
#11326 = EDGE_LOOP ( 'NONE', ( #7766, #1053, #7251, #11793 ) ) ;
#11327 = CARTESIAN_POINT ( 'NONE',  ( -25.01528890617809253, -10.29849948291661121, -14.47305271942837557 ) ) ;
#11328 = ORIENTED_EDGE ( 'NONE', *, *, #408, .F. ) ;
#11329 = CARTESIAN_POINT ( 'NONE',  ( 27.77288575766320378, -4.690764616287755651, -7.939653947423662039 ) ) ;
#11330 = ORIENTED_EDGE ( 'NONE', *, *, #3486, .T. ) ;
#11331 = CARTESIAN_POINT ( 'NONE',  ( 30.78070346053490880, -6.209293581256383199, -4.705209693361168455 ) ) ;
#11332 = CARTESIAN_POINT ( 'NONE',  ( -0.3208286057739646036, 4.433571671609678688, -0.3503314178412559321 ) ) ;
#11333 = DIRECTION ( 'NONE',  ( 0.9928203230275512992, 0.1196152422706614898, -0.000000000000000000 ) ) ;
#11334 = CARTESIAN_POINT ( 'NONE',  ( 27.18555652250208610, -2.580805812949960920, 4.533357778048667797 ) ) ;
#11335 = ORIENTED_EDGE ( 'NONE', *, *, #2895, .T. ) ;
#11336 = AXIS2_PLACEMENT_3D ( 'NONE', #143, #7409, #15278 ) ;
#11337 = CARTESIAN_POINT ( 'NONE',  ( 31.43732351782677625, -4.249272233123119413, -3.283357778048664688 ) ) ;
#11338 = CIRCLE ( 'NONE', #3554, 6.000000000000000888 ) ;
#11339 = DIRECTION ( 'NONE',  ( 0.1113444980252557837, -0.9937818688019538493, 0.000000000000000000 ) ) ;
#11340 = ORIENTED_EDGE ( 'NONE', *, *, #9289, .F. ) ;
#11341 = CARTESIAN_POINT ( 'NONE',  ( 26.20620856698912604, -7.060238655668615415, 7.033357778048657138 ) ) ;
#11342 = VECTOR ( 'NONE', #11739, 1000.000000000000000 ) ;
#11343 = ADVANCED_FACE ( 'NONE', ( #9924 ), #7231, .F. ) ;
#11344 = EDGE_CURVE ( 'NONE', #9029, #5484, #8773, .T. ) ;
#11345 = MECHANICAL_DESIGN_GEOMETRIC_PRESENTATION_REPRESENTATION (  '', ( #962 ), #2980 ) ;
#11346 = CARTESIAN_POINT ( 'NONE',  ( 27.00222791626931595, -2.275731535614434531, 5.783357778048668685 ) ) ;
#11347 = CARTESIAN_POINT ( 'NONE',  ( -18.05624385570398260, -20.06430210183123464, 15.83921756800030245 ) ) ;
#11348 = CARTESIAN_POINT ( 'NONE',  ( 2.500000000000000000, 2.357898499370432166, -2.385244779468109755E-15 ) ) ;
#11349 = ORIENTED_EDGE ( 'NONE', *, *, #1459, .F. ) ;
#11350 = CIRCLE ( 'NONE', #1251, 3.999999999999994671 ) ;
#11351 = LINE ( 'NONE', #13815, #3565 ) ;
#11352 = ORIENTED_EDGE ( 'NONE', *, *, #3204, .F. ) ;
#11353 = CARTESIAN_POINT ( 'NONE',  ( 25.71748644841968456, -2.420320648352046078, 5.783357778048663356 ) ) ;
#11354 = ORIENTED_EDGE ( 'NONE', *, *, #12851, .F. ) ;
#11355 = ADVANCED_FACE ( 'NONE', ( #15752 ), #17124, .F. ) ;
#11356 = CARTESIAN_POINT ( 'NONE',  ( 33.59503905791412137, -1.808589744724287129, -4.533357778048659803 ) ) ;
#11357 = CARTESIAN_POINT ( 'NONE',  ( 31.88017671309158274, -6.376637546091784792, -4.533357778048668685 ) ) ;
#11358 = VECTOR ( 'NONE', #2882, 1000.000000000000227 ) ;
#11359 = CARTESIAN_POINT ( 'NONE',  ( 0.000000000000000000, 0.000000000000000000, -10.47749643873921244 ) ) ;
#11360 = SHAPE_DEFINITION_REPRESENTATION ( #9387, #691 ) ;
#11361 = CARTESIAN_POINT ( 'NONE',  ( 29.65098506949083301, -2.583579140294649523, -4.705209693361160461 ) ) ;
#11362 = CARTESIAN_POINT ( 'NONE',  ( 33.56515079149260572, -5.873822666371450119, -6.861505862736167138 ) ) ;
#11363 = CARTESIAN_POINT ( 'NONE',  ( 41.54280399572520821, -0.01006661050770166557, -5.783357778048662468 ) ) ;
#11364 = CARTESIAN_POINT ( 'NONE',  ( 26.69778786461289855, -6.274106265784127778, -3.283357778048667797 ) ) ;
#11365 = STYLED_ITEM ( 'NONE', ( #17954 ), #17325 ) ;
#11366 = CARTESIAN_POINT ( 'NONE',  ( 30.80679339554874119, -2.444327062417882779, 4.705209693361168455 ) ) ;
#11367 = ORIENTED_EDGE ( 'NONE', *, *, #4209, .T. ) ;
#11368 = MANIFOLD_SOLID_BREP ( 'Thread1', #10420 ) ;
#11369 = EDGE_CURVE ( 'NONE', #4375, #2889, #5112, .T. ) ;
#11370 = EDGE_LOOP ( 'NONE', ( #989, #5631, #14204, #5396, #9673 ) ) ;
#11371 = CARTESIAN_POINT ( 'NONE',  ( 27.62849893492243325, -6.589071975465733644, 6.861505862736158257 ) ) ;
#11372 = FILL_AREA_STYLE ('',( #12744 ) ) ;
#11373 = CARTESIAN_POINT ( 'NONE',  ( 42.32364987186199556, -2.937684895442014277, -5.783357778048662468 ) ) ;
#11374 = ORIENTED_EDGE ( 'NONE', *, *, #11670, .T. ) ;
#11375 = SURFACE_SIDE_STYLE ('',( #5852 ) ) ;
#11376 = ORIENTED_EDGE ( 'NONE', *, *, #5256, .T. ) ;
#11377 = CYLINDRICAL_SURFACE ( 'NONE', #6370, 13.00000000000000178 ) ;
#11378 = ORIENTED_EDGE ( 'NONE', *, *, #5434, .F. ) ;
#11379 = CARTESIAN_POINT ( 'NONE',  ( 15.92260893619738837, -28.39189527176317540, -6.000000000000000000 ) ) ;
#11380 = DIRECTION ( 'NONE',  ( 0.8243186046180107640, 0.5661261679878571984, 0.000000000000000000 ) ) ;
#11381 = CARTESIAN_POINT ( 'NONE',  ( 0.000000000000000000, 0.000000000000000000, -12.00000000000000000 ) ) ;
#11382 = EDGE_CURVE ( 'NONE', #8560, #11271, #17426, .T. ) ;
#11383 = CARTESIAN_POINT ( 'NONE',  ( 26.66770885555339987, -3.370103022578743612, -8.283357778048658915 ) ) ;
#11384 = ORIENTED_EDGE ( 'NONE', *, *, #2220, .T. ) ;
#11385 = LINE ( 'NONE', #257, #10090 ) ;
#11386 = FACE_OUTER_BOUND ( 'NONE', #16248, .T. ) ;
#11387 = CARTESIAN_POINT ( 'NONE',  ( 32.56242593318007295, -2.859778545457410281, -7.939653947423660263 ) ) ;
#11388 = VERTEX_POINT ( 'NONE', #9034 ) ;
#11389 = VERTEX_POINT ( 'NONE', #14664 ) ;
#11390 = CARTESIAN_POINT ( 'NONE',  ( 25.94629020164262556, -4.319418220471658465, -8.066408332899133171 ) ) ;
#11391 = CARTESIAN_POINT ( 'NONE',  ( 26.66018910156667232, -2.644102211984857842, -4.533357778048659803 ) ) ;
#11392 = ORIENTED_EDGE ( 'NONE', *, *, #9449, .F. ) ;
#11393 = VERTEX_POINT ( 'NONE', #17222 ) ;
#11394 = ORIENTED_EDGE ( 'NONE', *, *, #10513, .T. ) ;
#11395 =( BOUNDED_CURVE ( )  B_SPLINE_CURVE ( 3, ( #4430, #8788, #14321, #17142 ),
 .UNSPECIFIED., .F., .T. ) 
 B_SPLINE_CURVE_WITH_KNOTS ( ( 4, 4 ),
 ( 4.846194975958193929, 4.967031014587541371 ),
 .UNSPECIFIED. ) 
 CURVE ( )  GEOMETRIC_REPRESENTATION_ITEM ( )  RATIONAL_B_SPLINE_CURVE ( ( 1.000000000000000000, 0.9987835910734579326, 0.9987835910734579326, 1.000000000000000000 ) ) 
 REPRESENTATION_ITEM ( '' )  );
#11396 = EDGE_LOOP ( 'NONE', ( #16155, #14957 ) ) ;
#11397 = CARTESIAN_POINT ( 'NONE',  ( 29.82181869931131146, -4.443908660051686610, 7.939653947423662039 ) ) ;
#11398 = ORIENTED_EDGE ( 'NONE', *, *, #13608, .T. ) ;
#11399 = CARTESIAN_POINT ( 'NONE',  ( 30.35023428074701002, -1.862166024106576057, -5.783357778048664244 ) ) ;
#11400 = CARTESIAN_POINT ( 'NONE',  ( 5.000000000000004441, 0.000000000000000000, 0.000000000000000000 ) ) ;
#11401 = PLANE ( 'NONE',  #11248 ) ;
#11402 = CARTESIAN_POINT ( 'NONE',  ( 32.90015225647083952, -1.554951264938056132, -5.113484796970854340 ) ) ;
#11403 = CARTESIAN_POINT ( 'NONE',  ( 31.67382807612511542, -6.101689702897060030, -6.861505862736167138 ) ) ;
#11404 = DIRECTION ( 'NONE',  ( -0.1196152422706611984, 0.9928203230275510771, 0.000000000000000000 ) ) ;
#11405 = DIRECTION ( 'NONE',  ( 0.000000000000000000, 0.000000000000000000, -1.000000000000000000 ) ) ;
#11406 = CARTESIAN_POINT ( 'NONE',  ( 0.000000000000000000, 0.000000000000000000, -2.000000000000000000 ) ) ;
#11407 = CARTESIAN_POINT ( 'NONE',  ( -3.248936832696171617, 17.78798921770683350, 17.00000000000000000 ) ) ;
#11408 = EDGE_CURVE ( 'NONE', #12324, #10066, #9551, .T. ) ;
#11409 = CARTESIAN_POINT ( 'NONE',  ( 31.08270050955629671, -4.291997302367946077, -3.627061608673664672 ) ) ;
#11410 = DIRECTION ( 'NONE',  ( -0.000000000000000000, -0.000000000000000000, 1.000000000000000000 ) ) ;
#11411 = CARTESIAN_POINT ( 'NONE',  ( 32.41296236253129592, -1.951006642345344044, -4.533357778048659803 ) ) ;
#11412 = CARTESIAN_POINT ( 'NONE',  ( 26.30054492745253825, -7.259773351106304951, -5.235134217867734030 ) ) ;
#11413 = CARTESIAN_POINT ( 'NONE',  ( 26.39379627684682106, -4.856917663858078882, 8.283357778048662468 ) ) ;
#11414 = CARTESIAN_POINT ( 'NONE',  ( 28.44643833274707845, -2.428894455266221275, 4.533357778048667797 ) ) ;
#11415 = CARTESIAN_POINT ( 'NONE',  ( 26.25801688195511474, -3.619335333876111171, -7.939653947423660263 ) ) ;
#11416 =( BOUNDED_CURVE ( )  B_SPLINE_CURVE ( 2, ( #16984, #4538, #4897, #7638, #10423, #13339, #14435, #17458, #4988, #920, #6454, #17555, #11784, #2290, #7808, #14624, #559, #13068, #15985, #4803, #4721, #7719, #2019, #6078, #13161, #10593, #5074, #16162, #17363, #12976, #9083, #17267, #13244, #11609, #10329, #17172, #3645, #10245, #2205, #3370, #8901, #3551, #3725, #10516, #6356, #824, #11878, #16077, #15793, #9250, #15884, #11971, #9167, #14709, #6264, #14793, #7452, #7544, #6175, #651, #11699, #739, #3459, #8989, #14534, #2115, #12052, #3989, #11032, #17814, #14878, #4176, #5513, #15142, #9338, #10676, #7901, #9675, #12328, #2385, #16505, #17639, #6617, #7986, #16423, #1660, #5332, #14959, #9587, #10940, #2544, #12245, #15048, #1358, #5159, #16348, #13521, #2726, #16250, #10855, #8069, #1189, #16596, #1279, #13696, #6881, #4076, #2465, #8248, #13779, #12410, #13435, #1014, #17727, #8164, #6539, #3822, #1094, #5248, #12147, #10768, #6706, #3908, #9420, #13606, #9505, #2635, #6800, #17893, #5424, #9854, #91, #4520, #9948, #12870, #1636, #11296, #14049, #16684, #456, #4437, #11115, #7169, #15409, #8421, #176, #5598 ),
 .UNSPECIFIED., .F., .T. ) 
 B_SPLINE_CURVE_WITH_KNOTS ( ( 3, 2, 2, 2, 2, 2, 2, 2, 2, 2, 2, 2, 2, 2, 2, 2, 2, 2, 2, 2, 2, 2, 2, 2, 2, 2, 2, 2, 2, 2, 2, 2, 2, 2, 2, 2, 2, 2, 2, 2, 2, 2, 2, 2, 2, 2, 2, 2, 2, 2, 2, 2, 2, 2, 2, 2, 2, 2, 2, 2, 2, 2, 2, 2, 2, 2, 2, 2, 2, 2, 2, 2, 2, 3 ),
 ( 0.000000000000000000, 0.01322951968774666726, 0.02645903937549333451, 0.03968855906324000177, 0.05291807875098666902, 0.06614759843873332934, 0.07937711812648000353, 0.09260663781422667773, 0.1058361575019733380, 0.1190656771897200122, 0.1322951968774666587, 0.1455247165652133190, 0.1587542362529600071, 0.1719837559407066396, 0.1852132756284533555, 0.1984427953162000158, 0.2116723150039466761, 0.2249018346916933364, 0.2381313543794400245, 0.2513608740671866570, 0.2645903937549333174, 0.2778199134426800332, 0.2910494331304266380, 0.3042789528181733538, 0.3175084725059200141, 0.3307379921936667300, 0.3439675118814132793, 0.3571970315691599951, 0.3704265512569067109, 0.3836560709446533712, 0.3968855906324000316, 0.4101151103201466364, 0.4233446300078933522, 0.4365741496956400125, 0.4498036693833866728, 0.4630331890711333331, 0.4762627087588800490, 0.4894922284466267093, 0.5027217481343733141, 0.5159512678221199744, 0.5291807875098666347, 0.5424103071976132950, 0.5556398268853600664, 0.5688693465731067267, 0.5820988662608532760, 0.5953283859485999363, 0.6085579056363467076, 0.6217874253240932569, 0.6350169450118400283, 0.6482464646995866886, 0.6614759843873334599, 0.6747055040750800092, 0.6879350237628265585, 0.7011645434505734409, 0.7143940631383199902, 0.7276235828260666505, 0.7408531025138134218, 0.7540826222015599711, 0.7673121418893067425, 0.7805416615770532918, 0.7937711812648000631, 0.8070007009525467234, 0.8202302206402932727, 0.8334597403280399330, 0.8466892600157867044, 0.8599187797035333647, 0.8731482993912800250, 0.8863778190790266853, 0.8996073387667733456, 0.9128368584545200060, 0.9260663781422666663, 0.9392958978300133266, 0.9525254175177600979, 0.9555550897579921932 ),
 .UNSPECIFIED. ) 
 CURVE ( )  GEOMETRIC_REPRESENTATION_ITEM ( )  RATIONAL_B_SPLINE_CURVE ( ( 1.000000000000000000, 0.8660254037844387076, 1.000000000000000000, 0.8660254037844387076, 1.000000000000000000, 0.8660254037844387076, 1.000000000000000000, 0.8660254037844387076, 1.000000000000000000, 0.8660254037844387076, 1.000000000000000000, 0.8660254037844387076, 1.000000000000000000, 0.8660254037844387076, 1.000000000000000000, 0.8660254037844387076, 1.000000000000000000, 0.8660254037844387076, 1.000000000000000000, 0.8660254037844387076, 1.000000000000000000, 0.8660254037844387076, 1.000000000000000000, 0.8660254037844387076, 1.000000000000000000, 0.8660254037844387076, 1.000000000000000000, 0.8660254037844387076, 1.000000000000000000, 0.8660254037844387076, 1.000000000000000000, 0.8660254037844387076, 1.000000000000000000, 0.8660254037844387076, 1.000000000000000000, 0.8660254037844387076, 1.000000000000000000, 0.8660254037844387076, 1.000000000000000000, 0.8660254037844387076, 1.000000000000000000, 0.8660254037844387076, 1.000000000000000000, 0.8660254037844387076, 1.000000000000000000, 0.8660254037844387076, 1.000000000000000000, 0.8660254037844387076, 1.000000000000000000, 0.8660254037844387076, 1.000000000000000000, 0.8660254037844387076, 1.000000000000000000, 0.8660254037844387076, 1.000000000000000000, 0.8660254037844387076, 1.000000000000000000, 0.8660254037844387076, 1.000000000000000000, 0.8660254037844387076, 1.000000000000000000, 0.8660254037844387076, 1.000000000000000000, 0.8660254037844387076, 1.000000000000000000, 0.8660254037844387076, 1.000000000000000000, 0.8660254037844387076, 1.000000000000000000, 0.8660254037844387076, 1.000000000000000000, 0.8660254037844387076, 1.000000000000000000, 0.8660254037844387076, 1.000000000000000000, 0.8660254037844387076, 1.000000000000000000, 0.8660254037844387076, 1.000000000000000000, 0.8660254037844387076, 1.000000000000000000, 0.8660254037844387076, 1.000000000000000000, 0.8660254037844387076, 1.000000000000000000, 0.8660254037844387076, 1.000000000000000000, 0.8660254037844387076, 1.000000000000000000, 0.8660254037844387076, 1.000000000000000000, 0.8660254037844387076, 1.000000000000000000, 0.8660254037844387076, 1.000000000000000000, 0.8660254037844387076, 1.000000000000000000, 0.8660254037844387076, 1.000000000000000000, 0.8660254037844387076, 1.000000000000000000, 0.8660254037844387076, 1.000000000000000000, 0.8660254037844387076, 1.000000000000000000, 0.8660254037844387076, 1.000000000000000000, 0.8660254037844387076, 1.000000000000000000, 0.8660254037844387076, 1.000000000000000000, 0.8660254037844387076, 1.000000000000000000, 0.8660254037844387076, 1.000000000000000000, 0.8660254037844387076, 1.000000000000000000, 0.8660254037844387076, 1.000000000000000000, 0.8660254037844387076, 1.000000000000000000, 0.8660254037844387076, 1.000000000000000000, 0.8660254037844387076, 1.000000000000000000, 0.8660254037844387076, 1.000000000000000000, 0.8660254037844387076, 1.000000000000000000, 0.8660254037844387076, 1.000000000000000000, 0.8660254037844387076, 1.000000000000000000, 0.8660254037844387076, 1.000000000000000000, 0.8660254037844387076, 1.000000000000000000, 0.8660254037844387076, 1.000000000000000000, 0.8660254037844387076, 1.000000000000000000, 0.8660254037844387076, 1.000000000000000000, 0.8660254037844387076, 1.000000000000000000, 0.9693186809021840933, 0.9526899265169710418 ) ) 
 REPRESENTATION_ITEM ( '' )  );
#11417 = EDGE_CURVE ( 'NONE', #9483, #6202, #3900, .T. ) ;
#11418 = VERTEX_POINT ( 'NONE', #7758 ) ;
#11419 = VERTEX_POINT ( 'NONE', #13290 ) ;
#11420 = CARTESIAN_POINT ( 'NONE',  ( 26.58890374069123652, -3.379597482641427231, 3.283357778048666464 ) ) ;
#11421 = ORIENTED_EDGE ( 'NONE', *, *, #1398, .T. ) ;
#11422 = ORIENTED_EDGE ( 'NONE', *, *, #4639, .F. ) ;
#11423 = CARTESIAN_POINT ( 'NONE',  ( -19.73861724507318627, -10.88265359452670644, -15.55811197012310743 ) ) ;
#11424 = ORIENTED_EDGE ( 'NONE', *, *, #11842, .F. ) ;
#11425 = CARTESIAN_POINT ( 'NONE',  ( 27.88665588685489993, -3.423116496867954162, -3.627061608673662008 ) ) ;
#11426 = ORIENTED_EDGE ( 'NONE', *, *, #10870, .T. ) ;
#11427 = EDGE_CURVE ( 'NONE', #10047, #10383, #17410, .T. ) ;
#11428 = CARTESIAN_POINT ( 'NONE',  ( 32.16857880351144416, -6.669052543620333395, -5.783357778048668685 ) ) ;
#11429 = VERTEX_POINT ( 'NONE', #6834 ) ;
#11430 = PLANE ( 'NONE',  #12190 ) ;
#11431 = CARTESIAN_POINT ( 'NONE',  ( 32.87199790123699472, -1.558343308739095656, -5.783357778048663356 ) ) ;
#11432 = LINE ( 'NONE', #3025, #15864 ) ;
#11433 = MANIFOLD_SOLID_BREP ( 'Cavity1', #15959 ) ;
#11434 = CARTESIAN_POINT ( 'NONE',  ( 31.87265695910486230, -5.650636735497883478, -8.283357778048662468 ) ) ;
#11435 = CARTESIAN_POINT ( 'NONE',  ( 29.08935247050201767, -2.014077381790315702, -5.783357778048658027 ) ) ;
#11436 = CARTESIAN_POINT ( 'NONE',  ( 31.91459173804834748, -5.445711903524953712, 7.939653947423658487 ) ) ;
#11437 = CARTESIAN_POINT ( 'NONE',  ( -4.024497503033519941, 2.323544716729378568, -3.272167766733379946 ) ) ;
#11438 = SURFACE_STYLE_FILL_AREA ( #11153 ) ;
#11439 = PLANE ( 'NONE',  #2021 ) ;
#11440 = ORIENTED_EDGE ( 'NONE', *, *, #1989, .F. ) ;
#11441 = DIRECTION ( 'NONE',  ( -0.000000000000000000, -0.000000000000000000, -1.000000000000000000 ) ) ;
#11442 = ORIENTED_EDGE ( 'NONE', *, *, #13539, .F. ) ;
#11443 = CARTESIAN_POINT ( 'NONE',  ( 25.11802603177690330, -19.03270077640483038, -0.5379818257722508434 ) ) ;
#11444 = CARTESIAN_POINT ( 'NONE',  ( 27.17934203385504333, -30.00000000000000355, 0.000000000000000000 ) ) ;
#11445 = ORIENTED_EDGE ( 'NONE', *, *, #7640, .F. ) ;
#11446 = VERTEX_POINT ( 'NONE', #6572 ) ;
#11447 = CARTESIAN_POINT ( 'NONE',  ( 26.66770885555339987, -3.370103022578743612, -8.283357778048660691 ) ) ;
#11448 = CARTESIAN_POINT ( 'NONE',  ( 33.52375369703867847, -2.544085015380856518, -8.283357778048658915 ) ) ;
#11449 = DIRECTION ( 'NONE',  ( -0.1196152422706610735, 0.9928203230275511881, 0.000000000000000000 ) ) ;
#11450 = CARTESIAN_POINT ( 'NONE',  ( 28.12379965168153362, -6.829206799398704675, 4.533357778048659803 ) ) ;
#11451 = SHAPE_DEFINITION_REPRESENTATION ( #12298, #1480 ) ;
#11452 = DIRECTION ( 'NONE',  ( 0.000000000000000000, 0.000000000000000000, 1.000000000000000000 ) ) ;
#11453 = CARTESIAN_POINT ( 'NONE',  ( 29.77797860222238313, -3.195249460342344250, -3.627061608673662008 ) ) ;
#11454 = CARTESIAN_POINT ( 'NONE',  ( 33.32855701603872234, -2.140504347050403045, -6.861505862736158257 ) ) ;
#11455 = DIRECTION ( 'NONE',  ( 0.9928203230275512992, 0.1196152422706614898, -0.000000000000000000 ) ) ;
#11456 = CARTESIAN_POINT ( 'NONE',  ( 33.10345976029034887, -2.594722134608779207, 8.283357778048666020 ) ) ;
#11457 = CARTESIAN_POINT ( 'NONE',  ( 29.34898802046944155, -4.500875419183088866, 7.939653947423662039 ) ) ;
#11458 = ORIENTED_EDGE ( 'NONE', *, *, #8133, .T. ) ;
#11459 = ORIENTED_EDGE ( 'NONE', *, *, #2930, .F. ) ;
#11460 = EDGE_CURVE ( 'NONE', #12849, #16241, #2673, .T. ) ;
#11461 = CARTESIAN_POINT ( 'NONE',  ( 26.46816385032927599, -3.594016774262162706, -3.627061608673662896 ) ) ;
#11462 = EDGE_LOOP ( 'NONE', ( #7006, #15129, #13313, #15885 ) ) ;
#11463 = CARTESIAN_POINT ( 'NONE',  ( 32.17274868998081416, -2.279756424927169345, 6.861505862736166250 ) ) ;
#11464 = DIRECTION ( 'NONE',  ( 0.000000000000000000, 0.000000000000000000, 1.000000000000000000 ) ) ;
#11465 = FACE_OUTER_BOUND ( 'NONE', #13816, .T. ) ;
#11466 = VERTEX_POINT ( 'NONE', #4212 ) ;
#11467 = CARTESIAN_POINT ( 'NONE',  ( -2.016448651773435938E-27, -20.49999999999999645, 13.00000000000000178 ) ) ;
#11468 = CARTESIAN_POINT ( 'NONE',  ( 0.000000000000000000, 0.000000000000000000, 12.00000000000000000 ) ) ;
#11469 = CARTESIAN_POINT ( 'NONE',  ( 3.861362476283256129, 2.629030857715989988, -3.371615880910371565 ) ) ;
#11470 = CARTESIAN_POINT ( 'NONE',  ( 3.999999999999999112, -1.539600717839008981, -3.000726591567081769 ) ) ;
#11471 = CARTESIAN_POINT ( 'NONE',  ( 33.30246708102489350, -5.905470865888903020, -4.705209693361168455 ) ) ;
#11472 = DIRECTION ( 'NONE',  ( 0.000000000000000000, 0.000000000000000000, -1.000000000000000000 ) ) ;
#11473 = DIRECTION ( 'NONE',  ( -0.000000000000000000, -0.000000000000000000, 1.000000000000000000 ) ) ;
#11474 = CARTESIAN_POINT ( 'NONE',  ( 32.04158527077989760, -6.057382223572642665, -4.705209693361168455 ) ) ;
#11475 = VERTEX_POINT ( 'NONE', #12283 ) ;
#11476 = EDGE_CURVE ( 'NONE', #5903, #317, #5288, .T. ) ;
#11477 = CARTESIAN_POINT ( 'NONE',  ( 28.58911057998038885, -6.046239229258517867, 8.283357778048660691 ) ) ;
#11478 = CARTESIAN_POINT ( 'NONE',  ( 29.75233713454258933, -1.544652646670201523, 5.783357778048668685 ) ) ;
#11479 = VERTEX_POINT ( 'NONE', #8282 ) ;
#11480 = EDGE_CURVE ( 'NONE', #11111, #17553, #7941, .T. ) ;
#11481 = CARTESIAN_POINT ( 'NONE',  ( 29.34898802046944155, -4.500875419183088866, -3.627061608673664672 ) ) ;
#11482 = VERTEX_POINT ( 'NONE', #13641 ) ;
#11483 = VERTEX_POINT ( 'NONE', #9543 ) ;
#11484 = CARTESIAN_POINT ( 'NONE',  ( 30.25533603959949502, -6.272589980291270351, 4.705209693361160461 ) ) ;
#11485 = DIRECTION ( 'NONE',  ( -0.3420201433256631618, 0.000000000000000000, 0.9396926207859104263 ) ) ;
#11486 = CIRCLE ( 'NONE', #16438, 10.50000000000000000 ) ;
#11487 = DIRECTION ( 'NONE',  ( -1.000000000000000000, 0.000000000000000000, -0.000000000000000000 ) ) ;
#11488 = CARTESIAN_POINT ( 'NONE',  ( -29.04317620846695647, -17.86624673319742840, -13.43120144060744003 ) ) ;
#11489 = CARTESIAN_POINT ( 'NONE',  ( 31.24031073583692475, -4.273008382657478954, -3.627061608673664672 ) ) ;
#11490 = CARTESIAN_POINT ( 'NONE',  ( 31.97277696464621854, -6.702839660918840536, -5.783357778048663356 ) ) ;
#11491 = CYLINDRICAL_SURFACE ( 'NONE', #5808, 2.500000000000001776 ) ;
#11492 = CARTESIAN_POINT ( 'NONE',  ( 29.71979337562451207, -1.938121702948446323, -5.783357778048664244 ) ) ;
#11493 = CARTESIAN_POINT ( 'NONE',  ( 0.000000000000000000, 0.000000000000000000, -10.47749643873921244 ) ) ;
#11494 = DIRECTION ( 'NONE',  ( -0.000000000000000000, -0.000000000000000000, 1.000000000000000000 ) ) ;
#11495 = EDGE_CURVE ( 'NONE', #4518, #60, #11074, .T. ) ;
#11496 = CARTESIAN_POINT ( 'NONE',  ( 26.03917326857634151, -4.899642733102906433, -3.627061608673664672 ) ) ;
#11497 = DIRECTION ( 'NONE',  ( -1.000000000000000000, -1.224646799147353207E-16, 0.000000000000000000 ) ) ;
#11498 = CARTESIAN_POINT ( 'NONE',  ( 33.23365877489121090, -6.550928303235100891, -5.783357778048663356 ) ) ;
#11499 = DIRECTION ( 'NONE',  ( 0.8660254037844329345, -0.5000000000000099920, 0.000000000000000000 ) ) ;
#11500 =( BOUNDED_CURVE ( )  B_SPLINE_CURVE ( 2, ( #13164, #9086, #15797, #7723, #6359, #7823, #13446, #13354, #17740 ),
 .UNSPECIFIED., .F., .T. ) 
 B_SPLINE_CURVE_WITH_KNOTS ( ( 3, 2, 2, 2, 3 ),
 ( 0.01923076923076924918, 0.02564102564102564014, 0.03846153846153846367, 0.05128205128205128027, 0.05769230769230770939 ),
 .UNSPECIFIED. ) 
 CURVE ( )  GEOMETRIC_REPRESENTATION_ITEM ( )  RATIONAL_B_SPLINE_CURVE ( ( 0.9330127018922194093, 0.9330127018922195203, 1.000000000000000000, 0.8660254037844387076, 1.000000000000000000, 0.8660254037844387076, 1.000000000000000000, 0.9330127018922190762, 0.9330127018922194093 ) ) 
 REPRESENTATION_ITEM ( '' )  );
#11501 = CARTESIAN_POINT ( 'NONE',  ( 26.02974819644417792, -2.720057890826728109, 7.033357778048666020 ) ) ;
#11502 = CARTESIAN_POINT ( 'NONE',  ( 28.09001152836989235, -6.106370808549102414, 3.283357778048663800 ) ) ;
#11503 = CARTESIAN_POINT ( 'NONE',  ( 27.12505156253147831, -7.276697974355292864, -5.783357778048668685 ) ) ;
#11504 = EDGE_CURVE ( 'NONE', #16771, #4820, #4068, .T. ) ;
#11505 = ORIENTED_EDGE ( 'NONE', *, *, #15334, .F. ) ;
#11506 = CARTESIAN_POINT ( 'NONE',  ( -10.50000000000000000, -1.591841644184202181E-21, -6.005572809000082835 ) ) ;
#11507 = ORIENTED_EDGE ( 'NONE', *, *, #9926, .F. ) ;
#11508 = EDGE_CURVE ( 'NONE', #12121, #13857, #12461, .T. ) ;
#11509 = CARTESIAN_POINT ( 'NONE',  ( 0.000000000000000000, 0.000000000000000000, -4.700000000000000178 ) ) ;
#11510 = ORIENTED_EDGE ( 'NONE', *, *, #14304, .T. ) ;
#11511 = AXIS2_PLACEMENT_3D ( 'NONE', #11297, #14329, #4259 ) ;
#11512 = CARTESIAN_POINT ( 'NONE',  ( 26.19678349485696955, -4.880653813392439311, -3.627061608673664672 ) ) ;
#11513 = TOROIDAL_SURFACE ( 'NONE', #2566, 10.40000000000000036, 0.9000000000000003553 ) ;
#11514 = CARTESIAN_POINT ( 'NONE',  ( 26.82722439997946395, -4.804698134550569044, -3.627061608673664672 ) ) ;
#11515 = EDGE_CURVE ( 'NONE', #13858, #4517, #1400, .T. ) ;
#11516 = CARTESIAN_POINT ( 'NONE',  ( 27.71165237056504438, -5.952083095804076684, -7.939653947423664704 ) ) ;
#11517 = ORIENTED_EDGE ( 'NONE', *, *, #1141, .T. ) ;
#11518 = DIRECTION ( 'NONE',  ( 0.9928203230275512992, 0.1196152422706614898, -0.000000000000000000 ) ) ;
#11519 = CARTESIAN_POINT ( 'NONE',  ( 28.91555989733679866, -4.553094948490599592, -3.283357778048664688 ) ) ;
#11520 = DIRECTION ( 'NONE',  ( 1.000000000000000000, 0.000000000000000000, 0.000000000000000000 ) ) ;
#11521 = ORIENTED_EDGE ( 'NONE', *, *, #3345, .F. ) ;
#11522 = CONICAL_SURFACE ( 'NONE', #1393, 3.999999999999998224, 0.8911886515913775009 ) ;
#11523 = CARTESIAN_POINT ( 'NONE',  ( 30.67935139548315604, -7.248220074880824981, -5.783357778048669573 ) ) ;
#11524 =( BOUNDED_SURFACE ( )  B_SPLINE_SURFACE ( 3, 2, ( 
 ( #12427, #12, #9519 ),
 ( #8180, #9434, #16519 ),
 ( #13621, #4189, #6549 ),
 ( #4095, #16266, #7997 ),
 ( #1108, #11051, #9603 ),
 ( #16613, #12065, #1374 ) ),
 .UNSPECIFIED., .F., .F., .T. ) 
 B_SPLINE_SURFACE_WITH_KNOTS ( ( 4, 2, 4 ),
 ( 3, 3 ),
 ( 0.02023740217035201530, 0.02269762987400599993, 0.02515785757765998457 ),
 ( 0.000000000000000000, 1.000000000000000000 ),
 .UNSPECIFIED. ) 
 GEOMETRIC_REPRESENTATION_ITEM ( )  RATIONAL_B_SPLINE_SURFACE ( (
 ( 1.000000000000000000, 0.8047781539129733597, 1.000000000000000000),
 ( 1.000000000000000000, 0.8123770319057486144, 1.000000000000000000),
 ( 1.000000000000000000, 0.8190663783056398861, 1.000000000000000000),
 ( 1.000000000000000000, 0.8192359702877524130, 1.000000000000000000),
 ( 1.000000000000000000, 0.8126134888419467295, 1.000000000000000000),
 ( 1.000000000000000000, 0.8047712368238109093, 1.000000000000000000) ) ) 
 REPRESENTATION_ITEM ( '' )  SURFACE ( )  );
#11525 = CARTESIAN_POINT ( 'NONE',  ( 31.92212620501791775, -6.708942077180482855, -6.453230759126470595 ) ) ;
#11526 = CARTESIAN_POINT ( 'NONE',  ( 32.54503264317084188, -5.369756224683081669, 7.939653947423658487 ) ) ;
#11527 = VECTOR ( 'NONE', #13838, 1000.000000000000227 ) ;
#11528 = ADVANCED_FACE ( 'NONE', ( #6657 ), #16635, .F. ) ;
#11529 = DIRECTION ( 'NONE',  ( -0.1196152422706610735, 0.9928203230275511881, 0.000000000000000000 ) ) ;
#11530 = CARTESIAN_POINT ( 'NONE',  ( -26.11936545685874833, -21.64910423302892895, 14.20663795870742696 ) ) ;
#11531 = FACE_OUTER_BOUND ( 'NONE', #2589, .T. ) ;
#11532 = ORIENTED_EDGE ( 'NONE', *, *, #8603, .T. ) ;
#11533 = CARTESIAN_POINT ( 'NONE',  ( 10.47816170930907553, -0.6768509389586216951, -6.005572809000082835 ) ) ;
#11534 = ORIENTED_EDGE ( 'NONE', *, *, #8787, .F. ) ;
#11535 = CARTESIAN_POINT ( 'NONE',  ( 7.666200962222337267, 6.158133996769685758, -2.333128398347827925 ) ) ;
#11536 = CARTESIAN_POINT ( 'NONE',  ( 34.91600907648203389, -11.88801210197604341, 11.56671555609732671 ) ) ;
#11537 = ORIENTED_EDGE ( 'NONE', *, *, #14065, .F. ) ;
#11538 = CYLINDRICAL_SURFACE ( 'NONE', #2676, 2.500000000000001776 ) ;
#11539 = CARTESIAN_POINT ( 'NONE',  ( 33.09223089549517738, -4.049888575955752579, -8.283357778048662468 ) ) ;
#11540 = CARTESIAN_POINT ( 'NONE',  ( 46.74613609540429593, -1.397631045209497103, -5.783357778048662468 ) ) ;
#11541 = EDGE_CURVE ( 'NONE', #8190, #15383, #7394, .T. ) ;
#11542 = DIRECTION ( 'NONE',  ( -0.01940847627338178338, 0.9998116377842107827, 1.665334536937734811E-16 ) ) ;
#11543 = CARTESIAN_POINT ( 'NONE',  ( 26.64639396487419987, -2.308405637095112706, -5.783357778048658027 ) ) ;
#11544 = DIRECTION ( 'NONE',  ( 0.9928203230275510771, 0.1196152422706614621, -0.000000000000000000 ) ) ;
#11545 = CARTESIAN_POINT ( 'NONE',  ( 2.500000000000000000, 2.253471898105738645E-15, 2.041999999999999815 ) ) ;
#11546 = DIRECTION ( 'NONE',  ( -0.1196152422706611984, 0.9928203230275510771, 0.000000000000000000 ) ) ;
#11547 = CARTESIAN_POINT ( 'NONE',  ( 31.56875459193803124, -6.114348982704044921, 6.861505862736157368 ) ) ;
#11548 = AXIS2_PLACEMENT_3D ( 'NONE', #14101, #1687, #7222 ) ;
#11549 = ORIENTED_EDGE ( 'NONE', *, *, #1129, .T. ) ;
#11550 = ORIENTED_EDGE ( 'NONE', *, *, #1899, .T. ) ;
#11551 = MANIFOLD_SOLID_BREP ( 'Sweep1', #10132 ) ;
#11552 = CIRCLE ( 'NONE', #7228, 6.000000000000000888 ) ;
#11553 = CARTESIAN_POINT ( 'NONE',  ( 38.43976950718546703, 0.6650622588958786663, -5.783357778048660691 ) ) ;
#11554 = ORIENTED_EDGE ( 'NONE', *, *, #2049, .F. ) ;
#11555 = EDGE_CURVE ( 'NONE', #10383, #10047, #11740, .T. ) ;
#11556 = CARTESIAN_POINT ( 'NONE',  ( 33.46007730730551799, -5.886481946178435010, 6.861505862736157368 ) ) ;
#11557 = CARTESIAN_POINT ( 'NONE',  ( 25.71748644841968456, -2.420320648352051851, -5.783357778048663356 ) ) ;
#11558 = DIRECTION ( 'NONE',  ( -0.1196152422706599494, 0.9928203230275514102, 0.000000000000000000 ) ) ;
#11559 = ADVANCED_FACE ( 'NONE', ( #6283 ), #13264, .F. ) ;
#11560 = VERTEX_POINT ( 'NONE', #12995 ) ;
#11561 = LINE ( 'NONE', #17129, #17534 ) ;
#11562 = DIRECTION ( 'NONE',  ( 1.000000000000000000, 0.000000000000000000, 0.000000000000000000 ) ) ;
#11563 = B_SPLINE_CURVE_WITH_KNOTS ( 'NONE', 3,
 ( #783, #611, #517, #10472, #4764, #4587 ),
 .UNSPECIFIED., .F., .F.,
 ( 4, 2, 4 ),
 ( 0.003358874760055540181, 0.004541967308452085107, 0.005725059856848630467 ),
 .UNSPECIFIED. ) ;
#11564 = LINE ( 'NONE', #5857, #8743 ) ;
#11565 = AXIS2_PLACEMENT_3D ( 'NONE', #3219, #4486, #10000 ) ;
#11566 = CARTESIAN_POINT ( 'NONE',  ( 26.66018910156667232, -2.644102211984857842, -4.533357778048659803 ) ) ;
#11567 = CARTESIAN_POINT ( 'NONE',  ( 25.37303892199676270, -2.799178389412888546, -7.033357778048658027 ) ) ;
#11568 = CARTESIAN_POINT ( 'NONE',  ( 28.29630561643014275, -19.54286113573893502, 13.63865706309495884 ) ) ;
#11569 = DIRECTION ( 'NONE',  ( -1.000000000000000000, 0.000000000000000000, 0.000000000000000000 ) ) ;
#11570 = SURFACE_STYLE_FILL_AREA ( #6041 ) ;
#11571 = CARTESIAN_POINT ( 'NONE',  ( 28.24571643650507369, -4.633797857156355171, -7.939653947423662039 ) ) ;
#11572 = AXIS2_PLACEMENT_3D ( 'NONE', #15756, #15387, #2974 ) ;
#11573 = FACE_OUTER_BOUND ( 'NONE', #8617, .T. ) ;
#11574 = CARTESIAN_POINT ( 'NONE',  ( 31.35480929215617252, -6.439933945126671055, 4.533357778048659803 ) ) ;
#11575 = VERTEX_POINT ( 'NONE', #4741 ) ;
#11576 = ORIENTED_EDGE ( 'NONE', *, *, #12652, .F. ) ;
#11577 = ORIENTED_EDGE ( 'NONE', *, *, #13189, .F. ) ;
#11578 = CARTESIAN_POINT ( 'NONE',  ( 26.34117031759772942, -2.982346454214467535, 6.861505862736165362 ) ) ;
#11579 = CARTESIAN_POINT ( 'NONE',  ( 0.000000000000000000, 0.000000000000000000, -2.000000000000000000 ) ) ;
#11580 = CARTESIAN_POINT ( 'NONE',  ( 20.00000000000000355, 7.999999999999996447, -6.000000000000000000 ) ) ;
#11581 = EDGE_CURVE ( 'NONE', #13923, #4502, #5838, .T. ) ;
#11582 = CARTESIAN_POINT ( 'NONE',  ( -8.876997858717690093, 16.38553564496311310, -16.83638096351226920 ) ) ;
#11583 = COLOUR_RGB ( '', 0.31764706, 0.68627451, 0.89019608) ;
#11584 = CARTESIAN_POINT ( 'NONE',  ( -17.70832741558421830, -19.55032950225749389, -15.89323616604937328 ) ) ;
#11585 = CARTESIAN_POINT ( 'NONE',  ( 32.19919549706052209, -6.038393303862174655, -4.705209693361169343 ) ) ;
#11586 = CARTESIAN_POINT ( 'NONE',  ( 30.35023428074701002, -1.862166024106576057, -5.783357778048664244 ) ) ;
#11587 = CARTESIAN_POINT ( 'NONE',  ( -19.43845002722867221, 2.988003976273734708, 0.000000000000000000 ) ) ;
#11588 = EDGE_LOOP ( 'NONE', ( #4237, #8067, #12161, #9317 ) ) ;
#11589 = CARTESIAN_POINT ( 'NONE',  ( 28.99436501219896201, -4.543600488427916417, -3.283357778048664688 ) ) ;
#11590 = LINE ( 'NONE', #4707, #7310 ) ;
#11591 = CARTESIAN_POINT ( 'NONE',  ( 26.07857582428556853, -4.894895503279006022, -8.283357778048662468 ) ) ;
#11592 = EDGE_CURVE ( 'NONE', #17243, #17459, #14459, .T. ) ;
#11593 = EDGE_LOOP ( 'NONE', ( #14802, #8511, #16661, #12325, #7550 ) ) ;
#11594 = CIRCLE ( 'NONE', #13057, 5.000000000000000000 ) ;
#11595 = ORIENTED_EDGE ( 'NONE', *, *, #12502, .F. ) ;
#11596 = CARTESIAN_POINT ( 'NONE',  ( 28.12741954877813555, -2.767138697495831856, -6.861505862736159145 ) ) ;
#11597 = CYLINDRICAL_SURFACE ( 'NONE', #9283, 2.500000000000001776 ) ;
#11598 = CARTESIAN_POINT ( 'NONE',  ( 35.46635924378174565, -16.45598204045931823, 11.37070560279563480 ) ) ;
#11599 = CARTESIAN_POINT ( 'NONE',  ( 26.17715024865825768, -6.235583268514400146, -3.900143082538624739 ) ) ;
#11600 = DIRECTION ( 'NONE',  ( -0.06446199418653550395, -0.9979201627913403261, -4.248110196704583871E-22 ) ) ;
#11601 = CIRCLE ( 'NONE', #2632, 12.50000000000000000 ) ;
#11602 =( GEOMETRIC_REPRESENTATION_CONTEXT ( 3 ) GLOBAL_UNCERTAINTY_ASSIGNED_CONTEXT ( ( #13740 ) ) GLOBAL_UNIT_ASSIGNED_CONTEXT ( ( #165, #15668, #15396 ) ) REPRESENTATION_CONTEXT ( 'NONE', 'WORKASPACE' ) );
#11603 = CARTESIAN_POINT ( 'NONE',  ( 30.04891049036066164, -7.324175753722694360, 5.783357778048657138 ) ) ;
#11604 = ORIENTED_EDGE ( 'NONE', *, *, #13283, .T. ) ;
#11605 = CARTESIAN_POINT ( 'NONE',  ( 32.32036211097666012, -1.624804527518282748, -5.783357778048663356 ) ) ;
#11606 = AXIS2_PLACEMENT_3D ( 'NONE', #14437, #3287, #13246 ) ;
#11607 = CIRCLE ( 'NONE', #9297, 5.000000000000000000 ) ;
#11608 = ORIENTED_EDGE ( 'NONE', *, *, #15671, .T. ) ;
#11609 = CARTESIAN_POINT ( 'NONE',  ( 32.16857880351144416, -6.669052543620333395, -5.783357778048668685 ) ) ;
#11610 = ORIENTED_EDGE ( 'NONE', *, *, #7546, .F. ) ;
#11611 = ADVANCED_FACE ( 'NONE', ( #6193 ), #6101, .F. ) ;
#11612 = DIRECTION ( 'NONE',  ( -1.000000000000000000, -0.000000000000000000, -0.000000000000000000 ) ) ;
#11613 = VERTEX_POINT ( 'NONE', #3579 ) ;
#11614 = CARTESIAN_POINT ( 'NONE',  ( 27.15566825608056689, -6.646038734597135011, -4.705209693361169343 ) ) ;
#11615 = CARTESIAN_POINT ( 'NONE',  ( 25.74134610602432360, -2.427642893298174620, -5.783357778048658027 ) ) ;
#11616 = EDGE_CURVE ( 'NONE', #13615, #16315, #5725, .T. ) ;
#11617 = CARTESIAN_POINT ( 'NONE',  ( 26.23609683341064525, -2.995005734021441768, -6.861505862736159145 ) ) ;
#11618 = CARTESIAN_POINT ( 'NONE',  ( 0.000000000000000000, 0.000000000000000000, -2.000000000000000000 ) ) ;
#11619 = CARTESIAN_POINT ( 'NONE',  ( 33.01342578063301403, -4.059383036018435753, -8.283357778048662468 ) ) ;
#11620 = FACE_BOUND ( 'NONE', #9903, .T. ) ;
#11621 = MECHANICAL_DESIGN_GEOMETRIC_PRESENTATION_REPRESENTATION (  '', ( #6420 ), #13944 ) ;
#11622 = CARTESIAN_POINT ( 'NONE',  ( 29.32081432955537892, -3.050456207659999475, -3.283357778048662023 ) ) ;
#11623 = CARTESIAN_POINT ( 'NONE',  ( 11.80000000000000249, 1.445083222993877036E-15, 0.000000000000000000 ) ) ;
#11624 = VERTEX_POINT ( 'NONE', #4822 ) ;
#11625 = CARTESIAN_POINT ( 'NONE',  ( 25.40682704530840397, -3.522014380262483702, 3.283357778048666464 ) ) ;
#11626 = AXIS2_PLACEMENT_3D ( 'NONE', #14515, #725, #13051 ) ;
#11627 = VECTOR ( 'NONE', #14262, 1000.000000000000227 ) ;
#11628 = ORIENTED_EDGE ( 'NONE', *, *, #13467, .T. ) ;
#11629 = VERTEX_POINT ( 'NONE', #10534 ) ;
#11630 = CARTESIAN_POINT ( 'NONE',  ( -10.50000000000000000, 0.000000000000000000, -4.000000000000000000 ) ) ;
#11631 = DIRECTION ( 'NONE',  ( -1.000000000000000000, 0.000000000000000000, 0.000000000000000000 ) ) ;
#11632 = CIRCLE ( 'NONE', #7585, 10.50000000000000000 ) ;
#11633 = ORIENTED_EDGE ( 'NONE', *, *, #710, .T. ) ;
#11634 = DIRECTION ( 'NONE',  ( 1.000000000000000000, 0.000000000000000000, 0.000000000000000000 ) ) ;
#11635 = ORIENTED_EDGE ( 'NONE', *, *, #1673, .T. ) ;
#11636 = CARTESIAN_POINT ( 'NONE',  ( 0.000000000000000000, 0.000000000000000000, -10.00000000000000000 ) ) ;
#11637 = LINE ( 'NONE', #16102, #4384 ) ;
#11638 = CARTESIAN_POINT ( 'NONE',  ( 10.50000000000000000, 1.285879139104720831E-15, -10.00000000000000000 ) ) ;
#11639 = AXIS2_PLACEMENT_3D ( 'NONE', #12300, #15011, #12205 ) ;
#11640 =( BOUNDED_CURVE ( )  B_SPLINE_CURVE ( 3, ( #12506, #8516, #4342, #5780 ),
 .UNSPECIFIED., .F., .T. ) 
 B_SPLINE_CURVE_WITH_KNOTS ( ( 4, 4 ),
 ( 3.141592653589793116, 6.283185307179586232 ),
 .UNSPECIFIED. ) 
 CURVE ( )  GEOMETRIC_REPRESENTATION_ITEM ( )  RATIONAL_B_SPLINE_CURVE ( ( 1.000000000000000000, 0.3333333333333333703, 0.3333333333333333703, 1.000000000000000000 ) ) 
 REPRESENTATION_ITEM ( '' )  );
#11641 = CARTESIAN_POINT ( 'NONE',  ( 29.75233713454258933, -1.544652646670201523, -5.783357778048658027 ) ) ;
#11642 = DIRECTION ( 'NONE',  ( -0.1196152422706620172, 0.9928203230275510771, 0.000000000000000000 ) ) ;
#11643 = DIRECTION ( 'NONE',  ( 0.9928203230275511881, 0.1196152422706610180, 9.614813431917825245E-17 ) ) ;
#11644 = CARTESIAN_POINT ( 'NONE',  ( 33.30663696749426350, -1.516174747195733863, -5.783357778048658027 ) ) ;
#11645 = EDGE_CURVE ( 'NONE', #4376, #9400, #15657, .T. ) ;
#11646 = CARTESIAN_POINT ( 'NONE',  ( -8.250000000000060396, -6.495190528383215423, -3.000000000000000000 ) ) ;
#11647 = CARTESIAN_POINT ( 'NONE',  ( 31.66250999073069750, -5.675955295111850596, -3.283357778048667797 ) ) ;
#11648 = CARTESIAN_POINT ( 'NONE',  ( 27.45766530510195835, -4.728742455708699666, 7.939653947423662039 ) ) ;
#11649 = APPLICATION_CONTEXT ( 'automotive_design' ) ;
#11650 = MECHANICAL_DESIGN_GEOMETRIC_PRESENTATION_REPRESENTATION (  '', ( #17506 ), #13415 ) ;
#11651 = ORIENTED_EDGE ( 'NONE', *, *, #4462, .T. ) ;
#11652 = CARTESIAN_POINT ( 'NONE',  ( 27.09860475545177039, -3.518061095420291995, -3.627061608673662896 ) ) ;
#11653 = ORIENTED_EDGE ( 'NONE', *, *, #11055, .F. ) ;
#11654 = CARTESIAN_POINT ( 'NONE',  ( 33.76207435632690590, -3.969185667289998332, 7.939653947423662039 ) ) ;
#11655 = DIRECTION ( 'NONE',  ( 1.000000000000000000, 0.000000000000000000, 0.000000000000000000 ) ) ;
#11656 = LINE ( 'NONE', #6496, #8189 ) ;
#11657 = EDGE_CURVE ( 'NONE', #1954, #14246, #9540, .T. ) ;
#11658 = ORIENTED_EDGE ( 'NONE', *, *, #6802, .F. ) ;
#11659 = CARTESIAN_POINT ( 'NONE',  ( 45.50000000000000000, -16.03270077640482683, 2.787981825772258837 ) ) ;
#11660 = VERTEX_POINT ( 'NONE', #15813 ) ;
#11662 = AXIS2_PLACEMENT_3D ( 'NONE', #2338, #9126, #14665 ) ;
#11661 = CARTESIAN_POINT ( 'NONE',  ( 2.804994570502172380, 3.229033611042450680, -3.226374918436836214 ) ) ;
#11663 = CARTESIAN_POINT ( 'NONE',  ( 33.32855701603872234, -2.140504347050403045, -6.861505862736158257 ) ) ;
#11664 = CARTESIAN_POINT ( 'NONE',  ( 25.96969170380761582, -2.000386719721422235, -5.783357778048658027 ) ) ;
#11665 = CARTESIAN_POINT ( 'NONE',  ( 28.75424055680402802, -6.753251120556833520, -7.033357778048666908 ) ) ;
#11666 = LINE ( 'NONE', #7951, #13601 ) ;
#11667 = FILL_AREA_STYLE_COLOUR ( '', #5354 ) ;
#11668 = CARTESIAN_POINT ( 'NONE',  ( 27.49697864365563760, -2.843094376337701679, -6.861505862736159145 ) ) ;
#11669 = EDGE_CURVE ( 'NONE', #1954, #11901, #13362, .T. ) ;
#11670 = EDGE_CURVE ( 'NONE', #43, #1615, #7566, .T. ) ;
#11671 = CARTESIAN_POINT ( 'NONE',  ( 32.47301885516785092, -2.670677813450649918, -3.283357778048662023 ) ) ;
#11672 = CARTESIAN_POINT ( 'NONE',  ( 29.81991338116587542, -2.990324628369393611, 3.283357778048666464 ) ) ;
#11673 = ORIENTED_EDGE ( 'NONE', *, *, #4632, .F. ) ;
#11674 = ORIENTED_EDGE ( 'NONE', *, *, #5451, .F. ) ;
#11675 = VERTEX_POINT ( 'NONE', #8832 ) ;
#11676 = CARTESIAN_POINT ( 'NONE',  ( 10.27627944162883544, 4.200961894323318013, -2.000000000000000000 ) ) ;
#11677 = CARTESIAN_POINT ( 'NONE',  ( 32.82963640218302004, -5.962437625020304388, 6.861505862736157368 ) ) ;
#11678 = DIRECTION ( 'NONE',  ( 0.000000000000000000, 0.000000000000000000, -1.000000000000000000 ) ) ;
#11679 = CARTESIAN_POINT ( 'NONE',  ( -12.26589791205140045, 14.78806204439702121, -16.57179146834700845 ) ) ;
#11680 = CARTESIAN_POINT ( 'NONE',  ( -16.75000000000000000, -16.63059030033399921, -16.03574476417184869 ) ) ;
#11681 = CARTESIAN_POINT ( 'NONE',  ( 32.17274868998081416, -2.279756424927169345, -4.705209693361160461 ) ) ;
#11682 = CARTESIAN_POINT ( 'NONE',  ( 33.18226487515251932, -2.585227674546096477, -3.283357778048662023 ) ) ;
#11683 = DIRECTION ( 'NONE',  ( 0.000000000000000000, 0.000000000000000000, -1.000000000000000000 ) ) ;
#11684 = CARTESIAN_POINT ( 'NONE',  ( -3.511755186886750479, 2.826662030176367413, -3.297382984111579596 ) ) ;
#11685 = CARTESIAN_POINT ( 'NONE',  ( 23.00000000000000000, -16.21813761408365195, -13.00000000000000178 ) ) ;
#11686 = PRODUCT_DEFINITION_CONTEXT ( 'detailed design', #13746, 'design' ) ;
#11687 = VERTEX_POINT ( 'NONE', #14368 ) ;
#11688 = ORIENTED_EDGE ( 'NONE', *, *, #6443, .T. ) ;
#11689 = EDGE_CURVE ( 'NONE', #5257, #1336, #1220, .T. ) ;
#11690 = CARTESIAN_POINT ( 'NONE',  ( 25.60565592828815440, -3.070961412863312034, -6.861505862736159145 ) ) ;
#11691 = DIRECTION ( 'NONE',  ( 0.000000000000000000, 0.000000000000000000, -1.000000000000000000 ) ) ;
#11692 = ORIENTED_EDGE ( 'NONE', *, *, #3515, .T. ) ;
#11693 = LINE ( 'NONE', #17263, #8336 ) ;
#11694 = EDGE_CURVE ( 'NONE', #9271, #8079, #671, .T. ) ;
#11695 = CARTESIAN_POINT ( 'NONE',  ( 29.86122125502053848, -4.439161430227785310, 3.283357778048664244 ) ) ;
#11696 = ORIENTED_EDGE ( 'NONE', *, *, #6840, .F. ) ;
#11697 = CARTESIAN_POINT ( 'NONE',  ( 29.40036258452792950, -7.012764792547963033, -6.453230759126474148 ) ) ;
#11698 = EDGE_CURVE ( 'NONE', #4061, #16943, #16511, .T. ) ;
#11699 = CARTESIAN_POINT ( 'NONE',  ( 30.45225960443380231, -4.367952981209816343, -3.627061608673664672 ) ) ;
#11700 = VERTEX_POINT ( 'NONE', #2565 ) ;
#11701 = DIRECTION ( 'NONE',  ( -0.000000000000000000, -0.000000000000000000, -1.000000000000000000 ) ) ;
#11702 = CARTESIAN_POINT ( 'NONE',  ( -35.19141017012124451, -14.17387298022714148, -11.46934516270795079 ) ) ;
#11703 = AXIS2_PLACEMENT_3D ( 'NONE', #16152, #8976, #17347 ) ;
#11704 = CARTESIAN_POINT ( 'NONE',  ( 29.69163902039066372, -1.941513746749485847, -6.453230759126468818 ) ) ;
#11705 = CARTESIAN_POINT ( 'NONE',  ( 27.62849893492243325, -6.589071975465733644, -4.705209693361168455 ) ) ;
#11706 = CARTESIAN_POINT ( 'NONE',  ( 21.42601376483257880, 2.765314980223224417, 0.000000000000000000 ) ) ;
#11707 = CARTESIAN_POINT ( 'NONE',  ( 27.33945763453056088, -4.742984145595265488, -8.283357778048662468 ) ) ;
#11708 = CARTESIAN_POINT ( 'NONE',  ( 27.49335874655903567, -6.905162478240574053, 4.533357778048659803 ) ) ;
#11709 = CARTESIAN_POINT ( 'NONE',  ( 27.84978555093622177, -3.227686124957687586, -8.283357778048658915 ) ) ;
#11710 = ADVANCED_FACE ( 'NONE', ( #10964 ), #3843, .F. ) ;
#11711 = DIRECTION ( 'NONE',  ( -0.000000000000000000, -0.000000000000000000, 1.000000000000000000 ) ) ;
#11712 = CARTESIAN_POINT ( 'NONE',  ( 31.30154412293507349, -3.011689903141150815, 3.627061608673666893 ) ) ;
#11713 = EDGE_CURVE ( 'NONE', #11286, #4257, #17171, .T. ) ;
#11714 = ORIENTED_EDGE ( 'NONE', *, *, #2046, .T. ) ;
#11715 = CARTESIAN_POINT ( 'NONE',  ( -31.74999999999995737, 0.000000000000000000, 0.000000000000000000 ) ) ;
#11716 = CARTESIAN_POINT ( 'NONE',  ( 8.632250723006720250, -18.84644399697197770, 13.00000000000000178 ) ) ;
#11717 = DIRECTION ( 'NONE',  ( -0.1196152422706610735, 0.9928203230275511881, 0.000000000000000000 ) ) ;
#11718 = VERTEX_POINT ( 'NONE', #14979 ) ;
#11719 = CARTESIAN_POINT ( 'NONE',  ( 26.31065902414478330, -7.328232685206446106, 5.254681170202263552 ) ) ;
#11720 = CARTESIAN_POINT ( 'NONE',  ( -10.47816170930907553, 0.6768509389586230274, -7.794427190999915211 ) ) ;
#11721 = CARTESIAN_POINT ( 'NONE',  ( 25.83973938098743517, -3.435034105423886874, -4.207126410816434792 ) ) ;
#11722 = CARTESIAN_POINT ( 'NONE',  ( 15.92260893619738837, -28.39189527176317540, -6.000000000000000000 ) ) ;
#11723 = CARTESIAN_POINT ( 'NONE',  ( 33.40745134805642635, -4.011910736534825439, 8.283357778048662468 ) ) ;
#11724 = ORIENTED_EDGE ( 'NONE', *, *, #7020, .F. ) ;
#11725 = CARTESIAN_POINT ( 'NONE',  ( 28.55903157092087952, -3.142235986053133256, -8.283357778048658915 ) ) ;
#11726 = CARTESIAN_POINT ( 'NONE',  ( -2.500000000000000000, 3.061616997868383141E-16, -10.00000000000000000 ) ) ;
#11727 = FACE_BOUND ( 'NONE', #5984, .T. ) ;
#11728 = CARTESIAN_POINT ( 'NONE',  ( 30.78487334700428590, -1.819997462563214263, -5.783357778048658027 ) ) ;
#11729 = EDGE_CURVE ( 'NONE', #10591, #6646, #878, .T. ) ;
#11730 = LINE ( 'NONE', #5025, #17785 ) ;
#11731 = DIRECTION ( 'NONE',  ( -0.9979201627913402151, 0.06446199418653550395, 5.311609029246448998E-22 ) ) ;
#11732 = CARTESIAN_POINT ( 'NONE',  ( 27.91310269393460430, -7.181753375802955475, 5.783357778048657138 ) ) ;
#11733 = ORIENTED_EDGE ( 'NONE', *, *, #17570, .F. ) ;
#11734 = ORIENTED_EDGE ( 'NONE', *, *, #8075, .F. ) ;
#11735 = CARTESIAN_POINT ( 'NONE',  ( 25.58373587974369201, -2.446631813008643075, -5.783357778048658027 ) ) ;
#11736 = VERTEX_POINT ( 'NONE', #9613 ) ;
#11737 = CARTESIAN_POINT ( 'NONE',  ( 32.95662993491455950, -6.574107945067995118, 5.783357778048657138 ) ) ;
#11738 = CARTESIAN_POINT ( 'NONE',  ( 28.19013153391124860, -7.158573733970061248, 5.783357778048669573 ) ) ;
#11739 = DIRECTION ( 'NONE',  ( 0.6174492339697391641, 0.7866107318554600436, 0.000000000000000000 ) ) ;
#11740 = B_SPLINE_CURVE_WITH_KNOTS ( 'NONE', 3,
 ( #410, #14178, #8650, #3117, #1769, #7029, #17099, #16820, #1865, #7298, #11347, #14088, #4475, #6001, #12721, #14004, #12817, #4652, #4387, #13903, #5914, #8748, #17004, #4558, #2842, #10080, #315, #2937, #8371, #11530, #15630, #12547, #1587, #7120, #3207, #14279, #9901, #15450, #3033, #8556, #1675, #16919, #5821 ),
 .UNSPECIFIED., .F., .F.,
 ( 4, 2, 2, 1, 2, 2, 2, 2, 2, 2, 2, 2, 2, 2, 2, 2, 2, 2, 2, 2, 2, 4 ),
 ( 0.01976914256504654077, 0.02100445419277401429, 0.02162211000663775626, 0.02223976582050150169, 0.02285742163436524366, 0.02347507744822898562, 0.02471038907595646955, 0.02594570070368395695, 0.02718101233141144435, 0.02779866814527519325, 0.02841632395913894216, 0.02965163558686643996, 0.03088694721459393777, 0.03150460302845767974, 0.03212225884232142170, 0.03335757047004890563, 0.03459288209777638956, 0.03582819372550387349, 0.03644584953936762239, 0.03706350535323135742, 0.03829881698095885523, 0.03953412860868634610 ),
 .UNSPECIFIED. ) ;
#11741 = ORIENTED_EDGE ( 'NONE', *, *, #419, .T. ) ;
#11742 = B_SPLINE_CURVE_WITH_KNOTS ( 'NONE', 3,
 ( #15315, #8423, #13959, #11582, #12773, #17151, #6155, #15587, #11679, #7524, #4699, #8604, #17249, #15501, #1823, #10227 ),
 .UNSPECIFIED., .F., .F.,
 ( 4, 2, 2, 2, 2, 2, 2, 4 ),
 ( 0.000000000000000000, 0.004966453901722449327, 0.007449680852583671388, 0.008691294328014282852, 0.009932907803444893449, 0.01489936170516735839, 0.01738258865602858652, 0.01986581560688981465 ),
 .UNSPECIFIED. ) ;
#11743 =( NAMED_UNIT ( * ) PLANE_ANGLE_UNIT ( ) SI_UNIT ( $, .RADIAN. ) );
#11744 = DIRECTION ( 'NONE',  ( 1.000000000000000000, 0.000000000000000000, 0.000000000000000000 ) ) ;
#11745 = ADVANCED_FACE ( 'NONE', ( #5355 ), #8992, .T. ) ;
#11746 = DIRECTION ( 'NONE',  ( 0.000000000000000000, 0.000000000000000000, 1.000000000000000000 ) ) ;
#11747 = CARTESIAN_POINT ( 'NONE',  ( 32.81641299864316608, -4.083119185552795294, -7.939653947423662039 ) ) ;
#11748 = CARTESIAN_POINT ( 'NONE',  ( 26.73899421642883567, -2.634607751922174224, -4.533357778048659803 ) ) ;
#11749 = DIRECTION ( 'NONE',  ( -0.1196152422706610735, 0.9928203230275511881, 0.000000000000000000 ) ) ;
#11750 = CARTESIAN_POINT ( 'NONE',  ( 39.47566789204768867, -7.933013952457433682, -5.783357778048662468 ) ) ;
#11751 =( NAMED_UNIT ( * ) PLANE_ANGLE_UNIT ( ) SI_UNIT ( $, .RADIAN. ) );
#11752 = CARTESIAN_POINT ( 'NONE',  ( 28.76238721243587193, -5.825490297734302381, -3.627061608673667781 ) ) ;
#11753 = EDGE_CURVE ( 'NONE', #14985, #9477, #6962, .T. ) ;
#11754 = DIRECTION ( 'NONE',  ( 0.000000000000000000, 1.000000000000000000, -1.224646799147353207E-16 ) ) ;
#11755 = CARTESIAN_POINT ( 'NONE',  ( 30.25524682244395436, -4.391689130744175884, 8.283357778048662468 ) ) ;
#11756 = ADVANCED_BREP_SHAPE_REPRESENTATION ( '', ( #11551, #3575 ), #10716 ) ;
#11757 = ORIENTED_EDGE ( 'NONE', *, *, #9997, .T. ) ;
#11758 = ORIENTED_EDGE ( 'NONE', *, *, #14955, .T. ) ;
#11759 = ORIENTED_EDGE ( 'NONE', *, *, #3542, .F. ) ;
#11760 = CARTESIAN_POINT ( 'NONE',  ( 3.678949249685231848, 0.000000000000000000, 0.000000000000000000 ) ) ;
#11761 = CARTESIAN_POINT ( 'NONE',  ( 33.33308377457396432, -5.274811626130743392, 7.939653947423658487 ) ) ;
#11762 = ORIENTED_EDGE ( 'NONE', *, *, #10374, .F. ) ;
#11763 = DIRECTION ( 'NONE',  ( 0.000000000000000000, 0.000000000000000000, -1.000000000000000000 ) ) ;
#11764 = DIRECTION ( 'NONE',  ( 1.000000000000000000, 0.000000000000000000, 0.000000000000000000 ) ) ;
#11765 = EDGE_CURVE ( 'NONE', #7873, #9123, #6553, .T. ) ;
#11766 = CARTESIAN_POINT ( 'NONE',  ( -21.42418507870700850, -22.26964835135415655, -15.24537475165205791 ) ) ;
#11767 = CARTESIAN_POINT ( 'NONE',  ( 27.65458886993626564, -2.824105456627233224, -6.861505862736158257 ) ) ;
#11768 = CARTESIAN_POINT ( 'NONE',  ( 32.97895737133300287, -1.545456804875373402, -5.113484796970854340 ) ) ;
#11769 = CYLINDRICAL_SURFACE ( 'NONE', #9006, 2.000000000000001776 ) ;
#11770 = VERTEX_POINT ( 'NONE', #16183 ) ;
#11771 = CARTESIAN_POINT ( 'NONE',  ( 15.39462056267347734, 12.71537873815137232, 16.22282132715419678 ) ) ;
#11772 = CARTESIAN_POINT ( 'NONE',  ( 27.53153627355490229, -7.237921456612971483, -5.113484796970862334 ) ) ;
#11773 = DIRECTION ( 'NONE',  ( 1.000000000000000000, 0.000000000000000000, 0.000000000000000000 ) ) ;
#11774 = EDGE_LOOP ( 'NONE', ( #13245, #8151, #13922, #1254 ) ) ;
#11775 = CARTESIAN_POINT ( 'NONE',  ( 27.30005507882132676, -4.747731375419166788, -3.627061608673664672 ) ) ;
#11776 = ADVANCED_FACE ( 'NONE', ( #1299 ), #6638, .F. ) ;
#11777 = CARTESIAN_POINT ( 'NONE',  ( 32.72003615946069743, -2.840789625746940938, -7.939653947423660263 ) ) ;
#11778 = ORIENTED_EDGE ( 'NONE', *, *, #16958, .F. ) ;
#11779 = CARTESIAN_POINT ( 'NONE',  ( 28.30694982360322953, -3.372479377640031473, -7.939653947423660263 ) ) ;
#11780 = CARTESIAN_POINT ( 'NONE',  ( 3.333333333333333925, -2.694301256218262886, -3.000726591567083545 ) ) ;
#11781 = DIRECTION ( 'NONE',  ( 0.9928203230275510771, 0.1196152422706614621, -0.000000000000000000 ) ) ;
#11782 = ORIENTED_EDGE ( 'NONE', *, *, #12527, .F. ) ;
#11783 = CARTESIAN_POINT ( 'NONE',  ( -4.000000000000000000, 2.309401076758501592, -3.133295621305381307 ) ) ;
#11784 = CARTESIAN_POINT ( 'NONE',  ( 32.97402322492378346, -4.064130265842336165, -3.627061608673664672 ) ) ;
#11785 = VERTEX_POINT ( 'NONE', #12166 ) ;
#11786 = EDGE_CURVE ( 'NONE', #8221, #10468, #6666, .T. ) ;
#11787 = CYLINDRICAL_SURFACE ( 'NONE', #8131, 2.100000000000000089 ) ;
#11788 = CARTESIAN_POINT ( 'NONE',  ( 28.05993251931039012, -3.202367565343740452, -3.283357778048662023 ) ) ;
#11789 = EDGE_LOOP ( 'NONE', ( #14862, #13114, #7330, #12993 ) ) ;
#11790 = AXIS2_PLACEMENT_3D ( 'NONE', #16976, #10567, #1927 ) ;
#11791 = CARTESIAN_POINT ( 'NONE',  ( 30.03080348965042745, -6.936809113706096319, -6.453230759126468818 ) ) ;
#11792 = CARTESIAN_POINT ( 'NONE',  ( 30.44283453230164227, -2.188368138933637574, -4.533357778048659803 ) ) ;
#11793 = ORIENTED_EDGE ( 'NONE', *, *, #14556, .T. ) ;
#11794 = CARTESIAN_POINT ( 'NONE',  ( 26.86653773853314320, -2.919050055179571945, -6.861505862736159145 ) ) ;
#11795 = EDGE_CURVE ( 'NONE', #15536, #16822, #16817, .T. ) ;
#11796 = CARTESIAN_POINT ( 'NONE',  ( 32.83754810739938534, -9.116730809865837060, -15.78335777804866424 ) ) ;
#11797 = CARTESIAN_POINT ( 'NONE',  ( 33.64386668575551198, -3.983427357176565486, -8.283357778048662468 ) ) ;
#11798 = DIRECTION ( 'NONE',  ( -0.000000000000000000, -0.000000000000000000, -1.000000000000000000 ) ) ;
#11799 = CARTESIAN_POINT ( 'NONE',  ( 26.58890374069123652, -3.379597482641427231, -8.283357778048658915 ) ) ;
#11800 = CARTESIAN_POINT ( 'NONE',  ( 31.51621784984448738, -6.120678622607529817, -6.861505862736166250 ) ) ;
#11801 = AXIS2_PLACEMENT_3D ( 'NONE', #9949, #16964, #3081 ) ;
#11802 = ORIENTED_EDGE ( 'NONE', *, *, #8574, .F. ) ;
#11803 = CARTESIAN_POINT ( 'NONE',  ( -15.92260893619738837, -28.39189527176317540, -6.000000000000000000 ) ) ;
#11804 = DIRECTION ( 'NONE',  ( 0.1113444980252557837, -0.9937818688019538493, 0.000000000000000000 ) ) ;
#11805 = VECTOR ( 'NONE', #1928, 1000.000000000000000 ) ;
#11806 = DIRECTION ( 'NONE',  ( 0.000000000000000000, 0.000000000000000000, -1.000000000000000000 ) ) ;
#11807 = VERTEX_POINT ( 'NONE', #13799 ) ;
#11808 = CARTESIAN_POINT ( 'NONE',  ( -7.499998387031003411, -20.49508120620799900, -12.00000000000000000 ) ) ;
#11809 = CARTESIAN_POINT ( 'NONE',  ( 31.00882954110335632, -1.782818301463667598, -5.113484796970851676 ) ) ;
#11810 = CARTESIAN_POINT ( 'NONE',  ( 25.75741033704265703, -2.751693534003876174, -5.973512092880350011 ) ) ;
#11811 = EDGE_CURVE ( 'NONE', #11466, #7755, #12072, .T. ) ;
#11812 = CARTESIAN_POINT ( 'NONE',  ( 32.80318959510331212, -2.203800746085299522, -4.705209693361160461 ) ) ;
#11813 = CARTESIAN_POINT ( 'NONE',  ( 30.10960860451258370, -6.927314653643411368, 5.113484796970852564 ) ) ;
#11814 = VECTOR ( 'NONE', #9499, 999.9999999999998863 ) ;
#11815 = CARTESIAN_POINT ( 'NONE',  ( 30.72436838703367812, -6.515889623968540434, -7.033357778048666908 ) ) ;
#11816 = CARTESIAN_POINT ( 'NONE',  ( -5.816800114226745675E-16, -4.862606272033100474, -3.445885042887441241 ) ) ;
#11817 = ITEM_DEFINED_TRANSFORMATION ( 'NONE', 'NONE', #7983,  #3575 ) ;
#11818 = CARTESIAN_POINT ( 'NONE',  ( 26.31556265977298992, -7.384422263489805793, -5.783357778048663356 ) ) ;
#11819 = DIRECTION ( 'NONE',  ( 1.000000000000000000, 3.552713678800500929E-15, 0.000000000000000000 ) ) ;
#11820 = CARTESIAN_POINT ( 'NONE',  ( 29.15206445563513071, -6.405512418264540209, -6.861505862736167138 ) ) ;
#11821 = VECTOR ( 'NONE', #1704, 1000.000000000000227 ) ;
#11822 = CARTESIAN_POINT ( 'NONE',  ( 32.52441275490655670, -6.636378442139655220, -5.783357778048663356 ) ) ;
#11823 = FACE_OUTER_BOUND ( 'NONE', #11247, .T. ) ;
#11824 = CARTESIAN_POINT ( 'NONE',  ( 33.45617745041539592, -1.098413033681664430, 5.783357778048668685 ) ) ;
#11825 = ORIENTED_EDGE ( 'NONE', *, *, #1512, .T. ) ;
#11826 = CARTESIAN_POINT ( 'NONE',  ( 26.30654288775393113, -7.309557114202775985, 6.143482903293868702 ) ) ;
#11827 = ORIENTED_EDGE ( 'NONE', *, *, #1689, .F. ) ;
#11828 = CARTESIAN_POINT ( 'NONE',  ( 32.69811611091622439, -2.216460025892273311, 4.705209693361168455 ) ) ;
#11829 = CARTESIAN_POINT ( 'NONE',  ( -19.73861724507318627, -10.88265359452670644, 15.55811197012310743 ) ) ;
#11830 = CARTESIAN_POINT ( 'NONE',  ( -8.776279441628885181, -6.799038105676576293, -11.72793873352920890 ) ) ;
#11831 = ORIENTED_EDGE ( 'NONE', *, *, #1543, .F. ) ;
#11832 =( NAMED_UNIT ( * ) SI_UNIT ( $, .STERADIAN. ) SOLID_ANGLE_UNIT ( ) );
#11833 = AXIS2_PLACEMENT_3D ( 'NONE', #1953, #9010, #11717 ) ;
#11834 = CARTESIAN_POINT ( 'NONE',  ( -15.92260893619738837, -28.39189527176317540, -6.000000000000000000 ) ) ;
#11835 = EDGE_CURVE ( 'NONE', #3411, #7377, #17830, .T. ) ;
#11836 = VERTEX_POINT ( 'NONE', #114 ) ;
#11837 = CARTESIAN_POINT ( 'NONE',  ( -34.91600907648203389, -11.88801210197604341, 12.00000000000000000 ) ) ;
#11838 = CARTESIAN_POINT ( 'NONE',  ( 33.56062403295735663, -2.739515387291124426, -3.627061608673662008 ) ) ;
#11839 = CARTESIAN_POINT ( 'NONE',  ( 31.41114436565740320, -6.133337902414513820, -4.705209693361168455 ) ) ;
#11840 = FACE_OUTER_BOUND ( 'NONE', #12762, .T. ) ;
#11841 = DIRECTION ( 'NONE',  ( -1.000000000000000000, -0.000000000000000000, -0.000000000000000000 ) ) ;
#11842 = EDGE_CURVE ( 'NONE', #12386, #227, #11138, .T. ) ;
#11843 = CARTESIAN_POINT ( 'NONE',  ( 29.64681518302145591, -6.972875258987813574, -5.783357778048668685 ) ) ;
#11844 = PRODUCT_DEFINITION_SHAPE ( 'NONE', 'NONE',  #1048 ) ;
#11845 = DIRECTION ( 'NONE',  ( 1.000000000000000000, 0.000000000000000000, 0.000000000000000000 ) ) ;
#11846 = CARTESIAN_POINT ( 'NONE',  ( 32.37175601071535880, -5.590505156207296267, 8.283357778048658915 ) ) ;
#11847 = AXIS2_PLACEMENT_3D ( 'NONE', #2787, #12484, #4239 ) ;
#11848 = EDGE_CURVE ( 'NONE', #11575, #12285, #8727, .T. ) ;
#11849 = ORIENTED_EDGE ( 'NONE', *, *, #2277, .F. ) ;
#11850 = ORIENTED_EDGE ( 'NONE', *, *, #1009, .T. ) ;
#11851 = CARTESIAN_POINT ( 'NONE',  ( 26.47269060886452507, -6.728324053342490174, 4.705209693361160461 ) ) ;
#11852 = VECTOR ( 'NONE', #17234, 1000.000000000000000 ) ;
#11853 = VECTOR ( 'NONE', #15805, 1000.000000000000114 ) ;
#11854 = CARTESIAN_POINT ( 'NONE',  ( 32.69811611091622439, -2.216460025892273311, 4.705209693361168455 ) ) ;
#11855 = ORIENTED_EDGE ( 'NONE', *, *, #10713, .F. ) ;
#11856 = DIRECTION ( 'NONE',  ( 1.000000000000000000, 0.000000000000000000, 0.000000000000000000 ) ) ;
#11857 = CARTESIAN_POINT ( 'NONE',  ( 25.17121605730381972, -3.996982838752419553, -5.783357778048664244 ) ) ;
#11858 = ADVANCED_FACE ( 'NONE', ( #14158 ), #393, .F. ) ;
#11859 = FACE_OUTER_BOUND ( 'NONE', #736, .T. ) ;
#11860 = CARTESIAN_POINT ( 'NONE',  ( 30.15443244188179150, -1.895953141405084086, -5.783357778048658027 ) ) ;
#11861 = CARTESIAN_POINT ( 'NONE',  ( 31.37049041475757605, -6.775403295959669947, -6.453230759126470595 ) ) ;
#11862 = CARTESIAN_POINT ( 'NONE',  ( 30.35023428074701002, -1.862166024106576057, -5.783357778048664244 ) ) ;
#11863 = CIRCLE ( 'NONE', #4047, 10.50000000000000000 ) ;
#11864 = CARTESIAN_POINT ( 'NONE',  ( 32.37175601071535880, -5.590505156207296267, -3.283357778048667797 ) ) ;
#11865 = LINE ( 'NONE', #13422, #6724 ) ;
#11866 = DIRECTION ( 'NONE',  ( -0.9979201627913402151, 0.06446199418653550395, 5.311609029246448998E-22 ) ) ;
#11867 = ORIENTED_EDGE ( 'NONE', *, *, #8641, .F. ) ;
#11868 = CARTESIAN_POINT ( 'NONE',  ( 27.49697864365563760, -2.843094376337701679, -6.861505862736159145 ) ) ;
#11869 = CARTESIAN_POINT ( 'NONE',  ( 33.56515079149260572, -5.873822666371450119, -6.861505862736167138 ) ) ;
#11870 = ORIENTED_EDGE ( 'NONE', *, *, #11018, .F. ) ;
#11871 = CIRCLE ( 'NONE', #4635, 6.249999999999996447 ) ;
#11872 = DIRECTION ( 'NONE',  ( -0.1196152422706610735, 0.9928203230275511881, 0.000000000000000000 ) ) ;
#11873 = ADVANCED_FACE ( 'NONE', ( #5621 ), #4370, .T. ) ;
#11874 = CARTESIAN_POINT ( 'NONE',  ( 26.70901672940806648, -4.818939824437135755, 3.283357778048664244 ) ) ;
#11875 = AXIS2_PLACEMENT_3D ( 'NONE', #6083, #10946, #1097 ) ;
#11876 = ORIENTED_EDGE ( 'NONE', *, *, #13004, .T. ) ;
#11877 = CARTESIAN_POINT ( 'NONE',  ( 29.06119811526816576, -2.017469425591354337, -6.453230759126464378 ) ) ;
#11878 = CARTESIAN_POINT ( 'NONE',  ( 31.41114436565740320, -6.133337902414513820, -4.705209693361168455 ) ) ;
#11879 = ORIENTED_EDGE ( 'NONE', *, *, #15803, .T. ) ;
#11880 = DIRECTION ( 'NONE',  ( -1.000000000000000000, 0.000000000000000000, 0.000000000000000000 ) ) ;
#11881 = MECHANICAL_DESIGN_GEOMETRIC_PRESENTATION_REPRESENTATION (  '', ( #10426 ), #4352 ) ;
#11882 = DIRECTION ( 'NONE',  ( 1.000000000000000000, 0.000000000000000000, 0.000000000000000000 ) ) ;
#11883 = ORIENTED_EDGE ( 'NONE', *, *, #1104, .T. ) ;
#11884 = AXIS2_PLACEMENT_3D ( 'NONE', #12863, #3251, #5680 ) ;
#11885 = DIRECTION ( 'NONE',  ( -1.000000000000000000, -1.065814103640150279E-14, 0.000000000000000000 ) ) ;
#11886 = CARTESIAN_POINT ( 'NONE',  ( 31.70371634254663817, -2.036456781249897485, -4.533357778048659803 ) ) ;
#11887 = TOROIDAL_SURFACE ( 'NONE', #14213, 12.70000000000000284, 0.9000000000000003553 ) ;
#11888 = CARTESIAN_POINT ( 'NONE',  ( 26.03917326857634151, -4.899642733102906433, -3.627061608673664672 ) ) ;
#11889 = DIRECTION ( 'NONE',  ( 0.000000000000000000, 0.000000000000000000, -1.000000000000000000 ) ) ;
#11890 = CARTESIAN_POINT ( 'NONE',  ( 32.51061761821408425, -6.300681867249914525, -4.533357778048668685 ) ) ;
#11891 = CARTESIAN_POINT ( 'NONE',  ( 1.390214784104990997, 4.043996922316214437, -3.202509183706264917 ) ) ;
#11892 = CARTESIAN_POINT ( 'NONE',  ( 27.87986455999572399, -6.131689368163069531, -3.283357778048667797 ) ) ;
#11893 = EDGE_CURVE ( 'NONE', #11629, #15856, #5898, .T. ) ;
#11894 = CARTESIAN_POINT ( 'NONE',  ( 32.97402322492378346, -4.064130265842336165, -3.627061608673664672 ) ) ;
#11895 = EDGE_CURVE ( 'NONE', #14407, #9693, #14221, .T. ) ;
#11896 = CIRCLE ( 'NONE', #16536, 10.50000000000000000 ) ;
#11897 = AXIS2_PLACEMENT_3D ( 'NONE', #14692, #7703, #10580 ) ;
#11898 = DIRECTION ( 'NONE',  ( 0.000000000000000000, 0.000000000000000000, -1.000000000000000000 ) ) ;
#11899 = CARTESIAN_POINT ( 'NONE',  ( 30.61929490284659394, -6.528548903775525325, -4.533357778048668685 ) ) ;
#11900 = CARTESIAN_POINT ( 'NONE',  ( 0.000000000000000000, 0.000000000000000000, 10.50000000000000000 ) ) ;
#11901 = VERTEX_POINT ( 'NONE', #8451 ) ;
#11902 = CARTESIAN_POINT ( 'NONE',  ( 26.10492286888474922, -5.636087676172644834, 3.446205193745024431 ) ) ;
#11903 = DIRECTION ( 'NONE',  ( -0.000000000000000000, -0.000000000000000000, -1.000000000000000000 ) ) ;
#11904 = CARTESIAN_POINT ( 'NONE',  ( 32.50119254608192421, -4.121097024973739309, -3.627061608673664672 ) ) ;
#11905 = CARTESIAN_POINT ( 'NONE',  ( 38.64694918415791136, -1.054552983374777098, -1.783357778048662912 ) ) ;
#11906 = CARTESIAN_POINT ( 'NONE',  ( 29.12189622942009493, -1.620608325512071568, -5.783357778048658027 ) ) ;
#11907 = DIRECTION ( 'NONE',  ( -0.1196152422706610735, 0.9928203230275511881, 0.000000000000000000 ) ) ;
#11908 = DIRECTION ( 'NONE',  ( -0.000000000000000000, -0.000000000000000000, 1.000000000000000000 ) ) ;
#11909 = CARTESIAN_POINT ( 'NONE',  ( 36.27615609941022257, -23.17738945083361557, 12.00000000000000000 ) ) ;
#11910 = CARTESIAN_POINT ( 'NONE',  ( 29.77797860222238313, -3.195249460342344250, -3.627061608673662008 ) ) ;
#11911 = CARTESIAN_POINT ( 'NONE',  ( 33.60446413004628141, -3.988174587000466342, -3.627061608673664672 ) ) ;
#11912 = CARTESIAN_POINT ( 'NONE',  ( 29.25000000000000000, -16.63088773646508756, -13.37255996287878013 ) ) ;
#11913 = CARTESIAN_POINT ( 'NONE',  ( 26.37178701114681800, -2.351687214456304353, 5.783357778048668685 ) ) ;
#11914 = ORIENTED_EDGE ( 'NONE', *, *, #1761, .F. ) ;
#11915 = EDGE_CURVE ( 'NONE', #5268, #7494, #10061, .T. ) ;
#11916 = CONICAL_SURFACE ( 'NONE', #4110, 2.041999999999999815, 1.047197551196591858 ) ;
#11917 = ORIENTED_EDGE ( 'NONE', *, *, #9974, .F. ) ;
#11918 = ORIENTED_EDGE ( 'NONE', *, *, #16812, .F. ) ;
#11919 = CARTESIAN_POINT ( 'NONE',  ( 30.18087924896149588, -5.654590020340094725, 7.939653947423658487 ) ) ;
#11920 = CARTESIAN_POINT ( 'NONE',  ( -29.20850947011023280, -15.38975055298431549, 13.38439523458337099 ) ) ;
#11921 = CARTESIAN_POINT ( 'NONE',  ( -10.40000000000000036, 0.000000000000000000, 0.000000000000000000 ) ) ;
#11922 = EDGE_CURVE ( 'NONE', #7124, #8890, #2911, .T. ) ;
#11923 = ORIENTED_EDGE ( 'NONE', *, *, #5296, .F. ) ;
#11924 = CARTESIAN_POINT ( 'NONE',  ( 33.01342578063301403, -4.059383036018435753, -8.283357778048662468 ) ) ;
#11925 = ORIENTED_EDGE ( 'NONE', *, *, #12421, .F. ) ;
#11926 = AXIS2_PLACEMENT_3D ( 'NONE', #8233, #13766, #17964 ) ;
#11927 = LINE ( 'NONE', #10382, #5197 ) ;
#11928 = FACE_BOUND ( 'NONE', #10009, .T. ) ;
#11929 = CARTESIAN_POINT ( 'NONE',  ( 32.18597209352066812, -4.159074864394664672, -7.939653947423662039 ) ) ;
#11930 = CARTESIAN_POINT ( 'NONE',  ( 32.12473870642251939, -5.420393343910986594, -7.939653947423664704 ) ) ;
#11931 = CARTESIAN_POINT ( 'NONE',  ( 28.72045243349238675, -6.030415129707233035, -8.283357778048664244 ) ) ;
#11932 = AXIS2_PLACEMENT_3D ( 'NONE', #5312, #8043, #17872 ) ;
#11933 = DIRECTION ( 'NONE',  ( -0.1196152422706611984, 0.9928203230275510771, 0.000000000000000000 ) ) ;
#11934 = CARTESIAN_POINT ( 'NONE',  ( 28.56093688906631911, -4.595820017735426255, -3.627061608673664672 ) ) ;
#11935 = DIRECTION ( 'NONE',  ( 1.000000000000000000, 0.000000000000000000, 0.000000000000000000 ) ) ;
#11936 = CARTESIAN_POINT ( 'NONE',  ( -25.74999999999998934, -16.21813761408365195, -13.00000000000000355 ) ) ;
#11937 = CARTESIAN_POINT ( 'NONE',  ( 32.92339180097568629, -5.524043937428110063, -3.283357778048667797 ) ) ;
#11938 = AXIS2_PLACEMENT_3D ( 'NONE', #12378, #13659, #1248 ) ;
#11939 = CARTESIAN_POINT ( 'NONE',  ( 26.94172295629870462, -6.971623697019761146, 4.533357778048659803 ) ) ;
#11940 =( BOUNDED_CURVE ( )  B_SPLINE_CURVE ( 2, ( #6158, #11682, #2274, #11768, #8970 ),
 .UNSPECIFIED., .F., .T. ) 
 B_SPLINE_CURVE_WITH_KNOTS ( ( 3, 2, 3 ),
 ( 0.000000000000000000, 0.01282051282051282007, 0.01923076923076924918 ),
 .UNSPECIFIED. ) 
 CURVE ( )  GEOMETRIC_REPRESENTATION_ITEM ( )  RATIONAL_B_SPLINE_CURVE ( ( 1.000000000000000000, 0.8660254037844387076, 1.000000000000000000, 0.9330127018922191873, 0.9330127018922194093 ) ) 
 REPRESENTATION_ITEM ( '' )  );
#11941 = AXIS2_PLACEMENT_3D ( 'NONE', #15063, #12611, #5261 ) ;
#11942 = EDGE_CURVE ( 'NONE', #14093, #1819, #9295, .T. ) ;
#11943 = ORIENTED_EDGE ( 'NONE', *, *, #659, .T. ) ;
#11944 = ORIENTED_EDGE ( 'NONE', *, *, #12752, .T. ) ;
#11945 = ORIENTED_EDGE ( 'NONE', *, *, #15067, .T. ) ;
#11946 = ORIENTED_EDGE ( 'NONE', *, *, #4448, .T. ) ;
#11947 = CARTESIAN_POINT ( 'NONE',  ( 26.24062359194589433, -6.129313013101782559, 7.939653947423658487 ) ) ;
#11948 = AXIS2_PLACEMENT_3D ( 'NONE', #6222, #17511, #14587 ) ;
#11949 = DIRECTION ( 'NONE',  ( -1.000000000000000000, 0.000000000000000000, 0.000000000000000000 ) ) ;
#11950 = EDGE_CURVE ( 'NONE', #13310, #1298, #15968, .T. ) ;
#11951 = VERTEX_POINT ( 'NONE', #17080 ) ;
#11952 = PRESENTATION_STYLE_ASSIGNMENT (( #17150 ) ) ;
#11953 = CARTESIAN_POINT ( 'NONE',  ( 29.77044413525282707, -1.932019286686802895, -6.453230759126468818 ) ) ;
#11954 = COLOUR_RGB ( '', 0.31764706, 0.68627451, 0.89019608) ;
#11955 = LINE ( 'NONE', #1263, #15983 ) ;
#11956 = CARTESIAN_POINT ( 'NONE',  ( 30.30787278169304244, -6.266260340387784566, -4.705209693361169343 ) ) ;
#11957 = CARTESIAN_POINT ( 'NONE',  ( -5.210193653659516369E-16, -4.647091401871165317, -3.272172305156515026 ) ) ;
#11958 = CARTESIAN_POINT ( 'NONE',  ( 32.58190297908952004, -5.565186596593329149, -8.283357778048662468 ) ) ;
#11959 = CARTESIAN_POINT ( 'NONE',  ( 26.64639396487419987, -2.308405637095112706, -5.783357778048658027 ) ) ;
#11960 = CARTESIAN_POINT ( 'NONE',  ( 25.88156304229571703, -4.918631652813365562, -7.939653947423662039 ) ) ;
#11961 = DIRECTION ( 'NONE',  ( -5.026720092345836698E-22, 4.581671729415424240E-22, -1.000000000000000000 ) ) ;
#11962 = CARTESIAN_POINT ( 'NONE',  ( 32.06767520579373354, -2.292415704734142690, -6.861505862736158257 ) ) ;
#11963 = AXIS2_PLACEMENT_3D ( 'NONE', #3358, #12963, #17257 ) ;
#11964 = CARTESIAN_POINT ( 'NONE',  ( 31.03886041246737548, -3.043338102658604161, -3.627061608673662008 ) ) ;
#11965 = EDGE_LOOP ( 'NONE', ( #11505, #4562, #2675, #10910 ) ) ;
#11966 = CARTESIAN_POINT ( 'NONE',  ( 2.000000000000002665, -3.464101615137751278, 0.000000000000000000 ) ) ;
#11967 = LINE ( 'NONE', #5071, #15972 ) ;
#11968 = AXIS2_PLACEMENT_3D ( 'NONE', #7279, #8816, #15336 ) ;
#11969 = EDGE_LOOP ( 'NONE', ( #10510, #14702, #1526, #2540 ) ) ;
#11970 = FACE_OUTER_BOUND ( 'NONE', #1331, .T. ) ;
#11971 = CARTESIAN_POINT ( 'NONE',  ( 30.62726312072365431, -1.838986382273682718, -5.783357778048658915 ) ) ;
#11972 = VERTEX_POINT ( 'NONE', #7454 ) ;
#11973 = CARTESIAN_POINT ( 'NONE',  ( 0.000000000000000000, 1.178949249685218081, 2.041999999999998483 ) ) ;
#11974 = CARTESIAN_POINT ( 'NONE',  ( 2.500000000000000000, 0.000000000000000000, 2.041999999999999815 ) ) ;
#11975 = CARTESIAN_POINT ( 'NONE',  ( 25.85239768453567777, -3.540099486550930763, 7.452613241158525526 ) ) ;
#11976 = CARTESIAN_POINT ( 'NONE',  ( -4.000000000000000000, -2.168404344971008868E-15, -2.842992957459234304 ) ) ;
#11977 = ADVANCED_FACE ( 'NONE', ( #15796, #10425 ), #4723, .F. ) ;
#11978 = CIRCLE ( 'NONE', #12267, 2.749999999999992895 ) ;
#11979 = CARTESIAN_POINT ( 'NONE',  ( 32.69820532807177216, -4.097360875439379768, -3.283357778048664688 ) ) ;
#11980 = VERTEX_POINT ( 'NONE', #4992 ) ;
#11981 = CARTESIAN_POINT ( 'NONE',  ( 32.56242593318007295, -2.859778545457410281, -7.939653947423660263 ) ) ;
#11982 = CARTESIAN_POINT ( 'NONE',  ( 26.13631296615022137, -5.896629108145342357, -3.732065232213778394 ) ) ;
#11983 = CARTESIAN_POINT ( 'NONE',  ( 0.000000000000000000, 0.000000000000000000, -3.000000000000000000 ) ) ;
#11984 = DIRECTION ( 'NONE',  ( 1.000000000000000000, 0.000000000000000000, 0.000000000000000000 ) ) ;
#11985 = CARTESIAN_POINT ( 'NONE',  ( 28.78802868011566929, -7.476087111406434893, -5.783357778048669573 ) ) ;
#11986 = CARTESIAN_POINT ( 'NONE',  ( 30.88125018618674034, -3.062327022369072171, -3.627061608673662896 ) ) ;
#11987 = ORIENTED_EDGE ( 'NONE', *, *, #14965, .T. ) ;
#11988 =( BOUNDED_CURVE ( )  B_SPLINE_CURVE ( 2, ( #12368, #17935, #12288, #2499, #1404, #10985, #2847, #4128, #1501 ),
 .UNSPECIFIED., .F., .T. ) 
 B_SPLINE_CURVE_WITH_KNOTS ( ( 3, 2, 2, 2, 3 ),
 ( 0.7500000000000000000, 0.7564102564102563875, 0.7692307692307692735, 0.7820512820512820484, 0.7884615384615384359 ),
 .UNSPECIFIED. ) 
 CURVE ( )  GEOMETRIC_REPRESENTATION_ITEM ( )  RATIONAL_B_SPLINE_CURVE ( ( 0.9330127018922194093, 0.9330127018922194093, 1.000000000000000000, 0.8660254037844387076, 1.000000000000000000, 0.8660254037844387076, 1.000000000000000000, 0.9330127018922194093, 0.9330127018922194093 ) ) 
 REPRESENTATION_ITEM ( '' )  );
#11989 = ORIENTED_EDGE ( 'NONE', *, *, #5209, .T. ) ;
#11990 = CARTESIAN_POINT ( 'NONE',  ( 30.66050125466253107, -2.889050389913576655, 8.283357778048666020 ) ) ;
#11991 = CARTESIAN_POINT ( 'NONE',  ( -27.17934203385504333, -30.00000000000000355, -12.00000000000000000 ) ) ;
#11992 = VERTEX_POINT ( 'NONE', #15987 ) ;
#11993 = PRODUCT ( 'Caliper Body Half', 'Caliper Body Half', '', ( #5653 ) ) ;
#11994 = DIRECTION ( 'NONE',  ( -0.000000000000000000, -0.000000000000000000, 1.000000000000000000 ) ) ;
#11995 = CARTESIAN_POINT ( 'NONE',  ( -3.538288549924106796, -15.34800872113743431, 13.00000000000000178 ) ) ;
#11996 = EDGE_CURVE ( 'NONE', #5005, #16638, #2735, .T. ) ;
#11997 = CARTESIAN_POINT ( 'NONE',  ( 32.84384354600314282, -1.561735352540135180, 5.113484796970859669 ) ) ;
#11998 = ORIENTED_EDGE ( 'NONE', *, *, #9088, .F. ) ;
#11999 = CARTESIAN_POINT ( 'NONE',  ( 27.92859066579839222, -3.218191664895003967, -8.283357778048658915 ) ) ;
#12000 = CARTESIAN_POINT ( 'NONE',  ( -3.861362476283255241, -2.629030857715999314, -3.371615880910374230 ) ) ;
#12001 = ITEM_DEFINED_TRANSFORMATION ( 'NONE', 'NONE', #14061,  #3575 ) ;
#12002 = FACE_BOUND ( 'NONE', #8324, .T. ) ;
#12003 = CARTESIAN_POINT ( 'NONE',  ( -10.40000000000000036, 0.000000000000000000, 0.000000000000000000 ) ) ;
#12004 = CARTESIAN_POINT ( 'NONE',  ( 31.69574812466957781, -6.726019302751734763, -5.783357778048669573 ) ) ;
#12005 = CARTESIAN_POINT ( 'NONE',  ( 33.17547354829333273, -5.293800545841212291, -3.627061608673667781 ) ) ;
#12006 = CARTESIAN_POINT ( 'NONE',  ( 27.12922144900085186, -2.887401855662130146, 6.861505862736166250 ) ) ;
#12007 = PRODUCT_RELATED_PRODUCT_CATEGORY ( 'part', '', ( #15045 ) ) ;
#12008 = ORIENTED_EDGE ( 'NONE', *, *, #8838, .T. ) ;
#12009 = SHAPE_REPRESENTATION ( 'o-rings series g_iso_O-ring 23.6x1.8-B-ISO 3601-1', ( #3575 ), #10716 ) ;
#12010 = CARTESIAN_POINT ( 'NONE',  ( 30.30787278169304244, -6.266260340387784566, 6.861505862736157368 ) ) ;
#12011 = CARTESIAN_POINT ( 'NONE',  ( -4.024497503033519941, -2.323544716729384785, -3.272167766733382166 ) ) ;
#12012 = ORIENTED_EDGE ( 'NONE', *, *, #7118, .F. ) ;
#12013 = CARTESIAN_POINT ( 'NONE',  ( 32.84384354600314282, -1.561735352540135180, -6.453230759126467042 ) ) ;
#12014 = PLANE ( 'NONE',  #7246 ) ;
#12015 = ADVANCED_FACE ( 'NONE', ( #2293 ), #16079, .T. ) ;
#12016 = DIRECTION ( 'NONE',  ( -0.000000000000000000, -0.000000000000000000, -1.000000000000000000 ) ) ;
#12017 = CARTESIAN_POINT ( 'NONE',  ( 31.54230778485832332, -2.355712103769039611, -4.705209693361160461 ) ) ;
#12018 = CARTESIAN_POINT ( 'NONE',  ( 31.38469755857769528, -2.374701023479507178, -4.705209693361161349 ) ) ;
#12019 = CARTESIAN_POINT ( 'NONE',  ( -0.5276476219778145627, 4.314164656930851827, -3.020318136128644859 ) ) ;
#12020 = CARTESIAN_POINT ( 'NONE',  ( 31.67744797322171735, -2.039621600994187656, -7.033357778048658027 ) ) ;
#12021 = DIRECTION ( 'NONE',  ( -1.000000000000000000, 0.000000000000000000, 0.000000000000000000 ) ) ;
#12022 = CARTESIAN_POINT ( 'NONE',  ( 32.32036211097666012, -1.624804527518282748, -5.783357778048663356 ) ) ;
#12023 = LINE ( 'NONE', #17527, #16184 ) ;
#12024 = CARTESIAN_POINT ( 'NONE',  ( 32.24155699611449677, -1.634298987580965923, -5.783357778048664244 ) ) ;
#12025 = CARTESIAN_POINT ( 'NONE',  ( 28.58911057998038530, -6.046239229258517867, 8.283357778048658915 ) ) ;
#12026 = ORIENTED_EDGE ( 'NONE', *, *, #7422, .F. ) ;
#12027 = EDGE_LOOP ( 'NONE', ( #1990, #68 ) ) ;
#12028 = ORIENTED_EDGE ( 'NONE', *, *, #5016, .T. ) ;
#12029 = CARTESIAN_POINT ( 'NONE',  ( 32.02836186724004364, -4.178063784105134459, 3.627061608673664228 ) ) ;
#12030 = CARTESIAN_POINT ( 'NONE',  ( 30.19827253897071273, -3.144612341114421561, 3.627061608673666449 ) ) ;
#12031 = ORIENTED_EDGE ( 'NONE', *, *, #2994, .F. ) ;
#12032 = CARTESIAN_POINT ( 'NONE',  ( 41.90164972253716513, -2.988527579590351646, -5.783357778048662468 ) ) ;
#12033 = CARTESIAN_POINT ( 'NONE',  ( 0.000000000000000000, 0.000000000000000000, -3.000000000000000000 ) ) ;
#12034 = CARTESIAN_POINT ( 'NONE',  ( -45.50000000000000000, -16.03270077640482683, 5.537981825772250843 ) ) ;
#12035 = CARTESIAN_POINT ( 'NONE',  ( 28.26310972651430120, -2.123820177930694442, -5.783357778048658027 ) ) ;
#12036 = CARTESIAN_POINT ( 'NONE',  ( 29.81239362717914787, -2.264323817775507397, 7.033357778048666020 ) ) ;
#12037 = VERTEX_POINT ( 'NONE', #4900 ) ;
#12039 = EDGE_CURVE ( 'NONE', #2012, #8375, #13054, .T. ) ;
#12038 = DIRECTION ( 'NONE',  ( 0.000000000000000000, 0.000000000000000000, -1.000000000000000000 ) ) ;
#12040 = DIRECTION ( 'NONE',  ( 1.000000000000000000, 0.000000000000000000, 0.000000000000000000 ) ) ;
#12041 = CARTESIAN_POINT ( 'NONE',  ( 26.39823381822651882, -6.110324093391315436, -3.627061608673668225 ) ) ;
#12042 = CARTESIAN_POINT ( 'NONE',  ( 18.06432791129289939, -12.37828432491873443, 15.83774382844986484 ) ) ;
#12043 = SURFACE_SIDE_STYLE ('',( #5148 ) ) ;
#12044 = CARTESIAN_POINT ( 'NONE',  ( 30.91186687973582536, -2.431667782610909434, -4.705209693361160461 ) ) ;
#12045 = CARTESIAN_POINT ( 'NONE',  ( 31.02146712245815507, -5.553315781884258229, -7.939653947423662927 ) ) ;
#12046 = VERTEX_POINT ( 'NONE', #10157 ) ;
#12047 = EDGE_CURVE ( 'NONE', #13311, #10072, #11003, .T. ) ;
#12048 = CARTESIAN_POINT ( 'NONE',  ( 35.62429925076629189, -17.76690233603958546, -10.53798182577225084 ) ) ;
#12049 = DIRECTION ( 'NONE',  ( -0.1196152422706584506, 0.9928203230275515212, 0.000000000000000000 ) ) ;
#12050 = EDGE_LOOP ( 'NONE', ( #7899, #7963, #16786, #13412 ) ) ;
#12051 = CARTESIAN_POINT ( 'NONE',  ( 32.51858583609114106, -1.611119345748072362, 5.783357778048668685 ) ) ;
#12052 = CARTESIAN_POINT ( 'NONE',  ( 30.13703915187255689, -4.405930820630744371, -7.939653947423662039 ) ) ;
#12053 = CARTESIAN_POINT ( 'NONE',  ( 0.000000000000000000, -1.178949249685213863, 2.042000000000001148 ) ) ;
#12054 = DIRECTION ( 'NONE',  ( -0.000000000000000000, -0.000000000000000000, 1.000000000000000000 ) ) ;
#12055 = CYLINDRICAL_SURFACE ( 'NONE', #15649, 2.499999999999999112 ) ;
#12056 = EDGE_CURVE ( 'NONE', #14281, #6423, #7641, .T. ) ;
#12057 = CARTESIAN_POINT ( 'NONE',  ( 29.70732014299206369, -2.276983097582480742, -7.033357778048658027 ) ) ;
#12058 = CARTESIAN_POINT ( 'NONE',  ( 30.93441382992541477, -1.402235749049144609, -5.783357778048658027 ) ) ;
#12059 = CIRCLE ( 'NONE', #14397, 13.60000000000000320 ) ;
#12060 = CARTESIAN_POINT ( 'NONE',  ( 33.38562051666750818, -5.268481986227246061, -7.939653947423664704 ) ) ;
#12061 = EDGE_CURVE ( 'NONE', #496, #2012, #17175, .T. ) ;
#12062 = CARTESIAN_POINT ( 'NONE',  ( 26.19644603989335963, -6.395740563884607432, -4.006386918492157889 ) ) ;
#12063 = DIRECTION ( 'NONE',  ( 0.000000000000000000, 0.000000000000000000, 1.000000000000000000 ) ) ;
#12064 = CARTESIAN_POINT ( 'NONE',  ( 4.175003227304314279, 2.208362916365298911, -3.169254239516210880 ) ) ;
#12065 = CARTESIAN_POINT ( 'NONE',  ( 0.1410420225375878522, -4.700232803196147557, -3.387027626239170530 ) ) ;
#12066 = AXIS2_PLACEMENT_3D ( 'NONE', #4207, #16539, #1310 ) ;
#12067 = CARTESIAN_POINT ( 'NONE',  ( 31.91459173804835103, -5.445711903524953712, -3.627061608673667781 ) ) ;
#12068 = EDGE_CURVE ( 'NONE', #8375, #16681, #7277, .T. ) ;
#12069 = ORIENTED_EDGE ( 'NONE', *, *, #16213, .T. ) ;
#12070 = ORIENTED_EDGE ( 'NONE', *, *, #11495, .F. ) ;
#12071 = CARTESIAN_POINT ( 'NONE',  ( -45.50000000000000000, -16.03270077640482683, 5.537981825772250843 ) ) ;
#12072 = LINE ( 'NONE', #1384, #11270 ) ;
#12073 = ORIENTED_EDGE ( 'NONE', *, *, #8160, .F. ) ;
#12074 = CARTESIAN_POINT ( 'NONE',  ( 25.76775864925887660, -2.837585720338236861, 5.127143661396867280 ) ) ;
#12075 = CARTESIAN_POINT ( 'NONE',  ( 27.82847066025702887, -2.165988739474055791, -5.783357778048658027 ) ) ;
#12076 = EDGE_CURVE ( 'NONE', #8906, #8079, #15672, .T. ) ;
#12077 = CARTESIAN_POINT ( 'NONE',  ( 32.95662993491456660, -6.574107945067995118, -5.783357778048669573 ) ) ;
#12078 = CARTESIAN_POINT ( 'NONE',  ( 4.000000000000000000, 2.309401076758498483, -3.133295621305380863 ) ) ;
#12079 = ORIENTED_EDGE ( 'NONE', *, *, #16115, .F. ) ;
#12080 = CARTESIAN_POINT ( 'NONE',  ( 25.47811240618384687, -2.786519109605914757, -4.533357778048659803 ) ) ;
#12081 = CARTESIAN_POINT ( 'NONE',  ( 2.500000000000000000, -1.768423874527824902, -1.020999999999998353 ) ) ;
#12082 = CARTESIAN_POINT ( 'NONE',  ( 31.61111609099199171, -1.710254666422835745, 5.783357778048665132 ) ) ;
#12083 = CARTESIAN_POINT ( 'NONE',  ( 9.099998387031005720, -19.29508120620799971, -16.81964500401478091 ) ) ;
#12084 = CARTESIAN_POINT ( 'NONE',  ( 30.43486631442457835, -6.877930660435475296, -5.783357778048669573 ) ) ;
#12085 = CARTESIAN_POINT ( 'NONE',  ( 26.14456121274580624, -5.685614013951941992, -8.283357778048664244 ) ) ;
#12086 = CARTESIAN_POINT ( 'NONE',  ( 32.26287188679368967, -2.695996373064596607, 3.283357778048666464 ) ) ;
#12087 = VERTEX_POINT ( 'NONE', #563 ) ;
#12088 =( BOUNDED_CURVE ( )  B_SPLINE_CURVE ( 2, ( #17904, #8342, #12257, #4092, #11047, #5526, #6990, #2903, #16435 ),
 .UNSPECIFIED., .F., .T. ) 
 B_SPLINE_CURVE_WITH_KNOTS ( ( 3, 2, 2, 2, 3 ),
 ( 0.6346153846153846922, 0.6410256410256410797, 0.6538461538461538547, 0.6666666666666666297, 0.6730769230769231282 ),
 .UNSPECIFIED. ) 
 CURVE ( )  GEOMETRIC_REPRESENTATION_ITEM ( )  RATIONAL_B_SPLINE_CURVE ( ( 0.9330127018922192983, 0.9330127018922198534, 1.000000000000000000, 0.8660254037844387076, 1.000000000000000000, 0.8660254037844387076, 1.000000000000000000, 0.9330127018922187432, 0.9330127018922192983 ) ) 
 REPRESENTATION_ITEM ( '' )  );
#12089 = AXIS2_PLACEMENT_3D ( 'NONE', #4551, #3109, #11520 ) ;
#12090 = ADVANCED_FACE ( 'NONE', ( #10519 ), #2022, .F. ) ;
#12091 = ORIENTED_EDGE ( 'NONE', *, *, #6673, .T. ) ;
#12092 = CARTESIAN_POINT ( 'NONE',  ( 28.39010325924584421, -2.735490497978389612, 6.861505862736166250 ) ) ;
#12093 = DIRECTION ( 'NONE',  ( -0.1196152422706598106, 0.9928203230275514102, 0.000000000000000000 ) ) ;
#12094 = CARTESIAN_POINT ( 'NONE',  ( -2.016448651773435938E-27, -20.49999999999999645, 17.00000000000000000 ) ) ;
#12095 = ORIENTED_EDGE ( 'NONE', *, *, #10851, .F. ) ;
#12096 = DIRECTION ( 'NONE',  ( -1.000000000000000000, 0.000000000000000000, 0.000000000000000000 ) ) ;
#12097 = TOROIDAL_SURFACE ( 'NONE', #4864, 2.700000000000000622, 0.2000000000000000111 ) ;
#12098 = DIRECTION ( 'NONE',  ( 0.000000000000000000, 1.000000000000000000, 0.000000000000000000 ) ) ;
#12099 = EDGE_CURVE ( 'NONE', #4757, #10267, #5152, .T. ) ;
#12100 = CARTESIAN_POINT ( 'NONE',  ( 27.92859066579839222, -3.218191664895003523, -8.283357778048660691 ) ) ;
#12101 = ADVANCED_FACE ( 'NONE', ( #14537 ), #11787, .F. ) ;
#12102 = CARTESIAN_POINT ( 'NONE',  ( 30.91186687973582536, -2.431667782610909434, -4.705209693361160461 ) ) ;
#12103 = ORIENTED_EDGE ( 'NONE', *, *, #8527, .T. ) ;
#12104 = AXIS2_PLACEMENT_3D ( 'NONE', #6882, #11116, #5514 ) ;
#12105 = CARTESIAN_POINT ( 'NONE',  ( 30.41656616297672500, -2.191532958677927745, -7.033357778048658027 ) ) ;
#12106 = CIRCLE ( 'NONE', #5436, 14.00000000000000178 ) ;
#12107 = DIRECTION ( 'NONE',  ( -1.000000000000000000, 0.000000000000000000, -0.000000000000000000 ) ) ;
#12108 = CARTESIAN_POINT ( 'NONE',  ( 27.12505156253147476, -7.276697974355294640, 5.783357778048658027 ) ) ;
#12109 = DIRECTION ( 'NONE',  ( 0.000000000000000000, 1.000000000000000000, 0.000000000000000000 ) ) ;
#12110 = CARTESIAN_POINT ( 'NONE',  ( -45.50000000000000000, -19.03270077640483038, -5.537981825772250843 ) ) ;
#12111 = CARTESIAN_POINT ( 'NONE',  ( 33.32855701603872234, -2.140504347050403045, 4.705209693361168455 ) ) ;
#12112 = AXIS2_PLACEMENT_3D ( 'NONE', #3156, #7248, #11194 ) ;
#12113 = CARTESIAN_POINT ( 'NONE',  ( 27.46709037723411839, -6.908327297984874882, 7.033357778048657138 ) ) ;
#12114 =( BOUNDED_CURVE ( )  B_SPLINE_CURVE ( 2, ( #2876, #16854, #12391, #14032, #12660, #5401, #10919, #4058, #9740 ),
 .UNSPECIFIED., .F., .T. ) 
 B_SPLINE_CURVE_WITH_KNOTS ( ( 3, 2, 2, 2, 3 ),
 ( 0.5192307692307692735, 0.5256410256410256610, 0.5384615384615384359, 0.5512820512820513219, 0.5576923076923077094 ),
 .UNSPECIFIED. ) 
 CURVE ( )  GEOMETRIC_REPRESENTATION_ITEM ( )  RATIONAL_B_SPLINE_CURVE ( ( 0.9330127018922192983, 0.9330127018922198534, 1.000000000000000000, 0.8660254037844387076, 1.000000000000000000, 0.8660254037844387076, 1.000000000000000000, 0.9330127018922194093, 0.9330127018922194093 ) ) 
 REPRESENTATION_ITEM ( '' )  );
#12115 = EDGE_CURVE ( 'NONE', #15769, #10379, #2069, .T. ) ;
#12116 = ORIENTED_EDGE ( 'NONE', *, *, #15055, .T. ) ;
#12117 = EDGE_CURVE ( 'NONE', #15522, #29, #10678, .T. ) ;
#12118 = VERTEX_POINT ( 'NONE', #9251 ) ;
#12119 = ORIENTED_EDGE ( 'NONE', *, *, #15355, .T. ) ;
#12120 = VECTOR ( 'NONE', #16666, 1000.000000000000114 ) ;
#12121 = VERTEX_POINT ( 'NONE', #9590 ) ;
#12122 = B_SPLINE_CURVE_WITH_KNOTS ( 'NONE', 3,
 ( #11407, #5793, #17064, #12781, #4446, #5884, #10046, #4617, #14242, #10141, #2373, #13508, #5147, #9070, #10666, #10413 ),
 .UNSPECIFIED., .F., .F.,
 ( 4, 2, 2, 2, 2, 2, 2, 4 ),
 ( 0.000000000000000000, 0.004966453901722449327, 0.007449680852583671388, 0.008691294328014282852, 0.009932907803444893449, 0.01489936170516735839, 0.01738258865602858652, 0.01986581560688981465 ),
 .UNSPECIFIED. ) ;
#12123 = CARTESIAN_POINT ( 'NONE',  ( 33.40754056521197413, -5.892811586081919906, 4.705209693361160461 ) ) ;
#12124 = CARTESIAN_POINT ( 'NONE',  ( 29.77797860222238313, -3.195249460342344250, 7.939653947423662927 ) ) ;
#12125 = EDGE_LOOP ( 'NONE', ( #12408, #3864, #17177, #17372 ) ) ;
#12126 = DIRECTION ( 'NONE',  ( 0.000000000000000000, 0.000000000000000000, -1.000000000000000000 ) ) ;
#12127 = CARTESIAN_POINT ( 'NONE',  ( 32.33415724766913257, -1.960501102408027219, 7.033357778048666020 ) ) ;
#12128 = FACE_OUTER_BOUND ( 'NONE', #928, .T. ) ;
#12129 = CARTESIAN_POINT ( 'NONE',  ( 29.56783163384821833, -3.220568019956291383, -7.939653947423660263 ) ) ;
#12130 =( BOUNDED_CURVE ( )  B_SPLINE_CURVE ( 2, ( #15411, #2805, #14051, #16425, #13781, #8330, #13863, #6707, #2997 ),
 .UNSPECIFIED., .F., .T. ) 
 B_SPLINE_CURVE_WITH_KNOTS ( ( 3, 2, 2, 2, 3 ),
 ( 0.1730769230769231004, 0.1794871794871794879, 0.1923076923076923184, 0.2051282051282051211, 0.2115384615384615641 ),
 .UNSPECIFIED. ) 
 CURVE ( )  GEOMETRIC_REPRESENTATION_ITEM ( )  RATIONAL_B_SPLINE_CURVE ( ( 0.9330127018922194093, 0.9330127018922196314, 1.000000000000000000, 0.8660254037844387076, 1.000000000000000000, 0.8660254037844387076, 1.000000000000000000, 0.9330127018922190762, 0.9330127018922194093 ) ) 
 REPRESENTATION_ITEM ( '' )  );
#12131 = EDGE_LOOP ( 'NONE', ( #8552, #3408 ) ) ;
#12132 = VECTOR ( 'NONE', #13192, 1000.000000000000000 ) ;
#12133 = CARTESIAN_POINT ( 'NONE',  ( 0.000000000000000000, 1.178949249685213863, -2.042000000000001148 ) ) ;
#12134 = CYLINDRICAL_SURFACE ( 'NONE', #10758, 2.499999999999999112 ) ;
#12135 = CARTESIAN_POINT ( 'NONE',  ( 26.63030083514515312, -6.709335133632020387, -6.861505862736167138 ) ) ;
#12136 = PLANE ( 'NONE',  #5576 ) ;
#12137 = AXIS2_PLACEMENT_3D ( 'NONE', #8372, #490, #7121 ) ;
#12138 = CARTESIAN_POINT ( 'NONE',  ( 30.81132015408399027, -5.578634341498224458, -3.627061608673668225 ) ) ;
#12139 = CARTESIAN_POINT ( 'NONE',  ( 32.70264286945147347, -5.350767304972614546, -3.627061608673668225 ) ) ;
#12140 = FACE_OUTER_BOUND ( 'NONE', #14259, .T. ) ;
#12141 = DIRECTION ( 'NONE',  ( -0.000000000000000000, -0.000000000000000000, -1.000000000000000000 ) ) ;
#12142 = AXIS2_PLACEMENT_3D ( 'NONE', #7602, #9305, #11933 ) ;
#12143 = ORIENTED_EDGE ( 'NONE', *, *, #1846, .F. ) ;
#12144 = EDGE_CURVE ( 'NONE', #15022, #4229, #5334, .T. ) ;
#12145 = VERTEX_POINT ( 'NONE', #1191 ) ;
#12146 = CARTESIAN_POINT ( 'NONE',  ( 31.08270050955629671, -4.291997302367946077, 7.939653947423662039 ) ) ;
#12147 = CARTESIAN_POINT ( 'NONE',  ( 27.50150540219088313, -5.977401655418041138, -3.627061608673667781 ) ) ;
#12148 = AXIS2_PLACEMENT_3D ( 'NONE', #15292, #7058, #8399 ) ;
#12149 = DIRECTION ( 'NONE',  ( 0.1196152422706621143, 0.9928203230275509661, 0.000000000000000000 ) ) ;
#12150 = LINE ( 'NONE', #14713, #8998 ) ;
#12151 = CARTESIAN_POINT ( 'NONE',  ( 28.19013153391124860, -7.158573733970061248, -5.783357778048657138 ) ) ;
#12152 = CARTESIAN_POINT ( 'NONE',  ( 30.40162818048570514, -5.827866652795590241, -3.283357778048667797 ) ) ;
#12153 = ORIENTED_EDGE ( 'NONE', *, *, #12382, .T. ) ;
#12154 = FACE_OUTER_BOUND ( 'NONE', #4364, .T. ) ;
#12155 = DIRECTION ( 'NONE',  ( -1.000000000000000000, 0.000000000000000000, 0.000000000000000000 ) ) ;
#12156 = FACE_OUTER_BOUND ( 'NONE', #13732, .T. ) ;
#12157 = CARTESIAN_POINT ( 'NONE',  ( 38.70301816123731697, -5.700001250565214228, -1.783357778048662690 ) ) ;
#12158 = CONICAL_SURFACE ( 'NONE', #15927, 2.001963570546863025, 0.9599310885968768137 ) ;
#12159 = DIRECTION ( 'NONE',  ( -1.000000000000000000, 0.000000000000000000, 0.000000000000000000 ) ) ;
#12160 = EDGE_CURVE ( 'NONE', #1847, #9483, #8876, .T. ) ;
#12161 = ORIENTED_EDGE ( 'NONE', *, *, #12144, .T. ) ;
#12162 = AXIS2_PLACEMENT_3D ( 'NONE', #1952, #10352, #13180 ) ;
#12163 = VECTOR ( 'NONE', #17297, 1000.000000000000000 ) ;
#12164 = PLANE ( 'NONE',  #102 ) ;
#12165 = ORIENTED_EDGE ( 'NONE', *, *, #3067, .F. ) ;
#12166 = CARTESIAN_POINT ( 'NONE',  ( -5.384454397937117776, 6.702023979852544604E-16, -4.700000000000000178 ) ) ;
#12167 = EDGE_CURVE ( 'NONE', #11388, #8115, #10770, .T. ) ;
#12168 = ORIENTED_EDGE ( 'NONE', *, *, #2101, .F. ) ;
#12169 = SURFACE_STYLE_FILL_AREA ( #1119 ) ;
#12170 = EDGE_CURVE ( 'NONE', #4780, #2226, #7987, .T. ) ;
#12171 = VECTOR ( 'NONE', #17643, 1000.000000000000000 ) ;
#12172 = CARTESIAN_POINT ( 'NONE',  ( 32.70264286945147347, -5.350767304972614546, -3.627061608673668225 ) ) ;
#12173 =( GEOMETRIC_REPRESENTATION_CONTEXT ( 3 ) GLOBAL_UNCERTAINTY_ASSIGNED_CONTEXT ( ( #1733 ) ) GLOBAL_UNIT_ASSIGNED_CONTEXT ( ( #3980, #15128, #8238 ) ) REPRESENTATION_CONTEXT ( 'NONE', 'WORKASPACE' ) );
#12174 = CARTESIAN_POINT ( 'NONE',  ( 4.101954839143060916, 2.368264730582929634, -3.381130640444268032 ) ) ;
#12175 = CARTESIAN_POINT ( 'NONE',  ( 32.64557936882268052, -2.222789665795767089, -4.705209693361161349 ) ) ;
#12176 = VECTOR ( 'NONE', #12330, 1000.000000000000114 ) ;
#12177 = CARTESIAN_POINT ( 'NONE',  ( 31.63243098167119172, -2.771952051906466430, 3.283357778048666464 ) ) ;
#12178 = FACE_OUTER_BOUND ( 'NONE', #1935, .T. ) ;
#12179 = CIRCLE ( 'NONE', #4354, 0.2000000000000000944 ) ;
#12180 = CARTESIAN_POINT ( 'NONE',  ( 27.67650891848073158, -3.448435056481901295, -7.939653947423660263 ) ) ;
#12181 = CARTESIAN_POINT ( 'NONE',  ( 33.50243880635947846, -1.482387629897225390, 5.783357778048663356 ) ) ;
#12182 = CARTESIAN_POINT ( 'NONE',  ( 32.69820532807177216, -4.097360875439379768, 8.283357778048662468 ) ) ;
#12183 = ORIENTED_EDGE ( 'NONE', *, *, #1716, .T. ) ;
#12184 = VECTOR ( 'NONE', #6889, 1000.000000000000227 ) ;
#12185 = CARTESIAN_POINT ( 'NONE',  ( 30.60986983071443390, -4.348964061499348333, 7.939653947423662039 ) ) ;
#12186 = DIRECTION ( 'NONE',  ( 1.000000000000000000, 0.000000000000000000, 0.000000000000000000 ) ) ;
#12187 = CARTESIAN_POINT ( 'NONE',  ( 28.72045243349238675, -6.030415129707233035, 3.283357778048663356 ) ) ;
#12188 = AXIS2_PLACEMENT_3D ( 'NONE', #3911, #6540, #922 ) ;
#12189 = ORIENTED_EDGE ( 'NONE', *, *, #17178, .F. ) ;
#12190 = AXIS2_PLACEMENT_3D ( 'NONE', #15804, #4813, #14266 ) ;
#12191 = DIRECTION ( 'NONE',  ( 1.000000000000000000, 0.000000000000000000, 0.000000000000000000 ) ) ;
#12192 = ORIENTED_EDGE ( 'NONE', *, *, #15299, .T. ) ;
#12193 = DIRECTION ( 'NONE',  ( -0.1196152422706610735, 0.9928203230275511881, 0.000000000000000000 ) ) ;
#12194 = EDGE_LOOP ( 'NONE', ( #7402, #9972, #11291, #5817 ) ) ;
#12195 = CARTESIAN_POINT ( 'NONE',  ( 33.95908713831676096, -3.945449517755638791, -3.283357778048664688 ) ) ;
#12196 = CARTESIAN_POINT ( 'NONE',  ( 29.03376756790819613, -4.538853258604016006, -7.939653947423662039 ) ) ;
#12197 = VECTOR ( 'NONE', #9323, 999.9999999999998863 ) ;
#12198 = EDGE_CURVE ( 'NONE', #2203, #4586, #5426, .T. ) ;
#12199 = DIRECTION ( 'NONE',  ( -0.1196152422706624058, 0.9928203230275510771, 0.000000000000000000 ) ) ;
#12200 = CARTESIAN_POINT ( 'NONE',  ( -2.016448651773435938E-27, -20.49999999999999645, -13.00000000000000178 ) ) ;
#12201 = DIRECTION ( 'NONE',  ( 0.9979201627913405481, -0.06446199418653551783, -5.311609029246448998E-22 ) ) ;
#12202 = CARTESIAN_POINT ( 'NONE',  ( 26.87106449706838873, -6.053357334259913181, 7.939653947423658487 ) ) ;
#12203 =( BOUNDED_CURVE ( )  B_SPLINE_CURVE ( 2, ( #3206, #14278, #1864, #5178, #6978, #11990, #2402, #13862, #6477 ),
 .UNSPECIFIED., .F., .T. ) 
 B_SPLINE_CURVE_WITH_KNOTS ( ( 3, 2, 2, 2, 3 ),
 ( 0.2884615384615384914, 0.2948717948717948789, 0.3076923076923077094, 0.3205128205128205399, 0.3269230769230769273 ),
 .UNSPECIFIED. ) 
 CURVE ( )  GEOMETRIC_REPRESENTATION_ITEM ( )  RATIONAL_B_SPLINE_CURVE ( ( 0.9330127018922194093, 0.9330127018922196314, 1.000000000000000000, 0.8660254037844387076, 1.000000000000000000, 0.8660254037844387076, 1.000000000000000000, 0.9330127018922194093, 0.9330127018922194093 ) ) 
 REPRESENTATION_ITEM ( '' )  );
#12204 = CARTESIAN_POINT ( 'NONE',  ( 29.64681518302145591, -6.972875258987813574, 5.783357778048658027 ) ) ;
#12205 = DIRECTION ( 'NONE',  ( -0.1196152422706610735, 0.9928203230275511881, 0.000000000000000000 ) ) ;
#12206 = CARTESIAN_POINT ( 'NONE',  ( 32.52441275490655670, -6.636378442139655220, 5.783357778048664244 ) ) ;
#12207 = CARTESIAN_POINT ( 'NONE',  ( 32.28234893270314387, -5.401404424200516807, 3.627061608673662896 ) ) ;
#12208 = VECTOR ( 'NONE', #15422, 1000.000000000000000 ) ;
#12209 = CARTESIAN_POINT ( 'NONE',  ( 27.86101441917510257, -1.772519683195811657, 5.783357778048668685 ) ) ;
#12210 = ADVANCED_FACE ( 'NONE', ( #9507 ), #9005, .T. ) ;
#12211 = ORIENTED_EDGE ( 'NONE', *, *, #14243, .F. ) ;
#12212 = AXIS2_PLACEMENT_3D ( 'NONE', #14119, #15759, #1622 ) ;
#12213 = AXIS2_PLACEMENT_3D ( 'NONE', #8006, #11063, #4109 ) ;
#12214 = TOROIDAL_SURFACE ( 'NONE', #2389, 10.40000000000000036, 0.9000000000000003553 ) ;
#12215 = ORIENTED_EDGE ( 'NONE', *, *, #6529, .F. ) ;
#12216 = CARTESIAN_POINT ( 'NONE',  ( 31.08270050955629671, -4.291997302367946077, 7.939653947423662039 ) ) ;
#12217 = CARTESIAN_POINT ( 'NONE',  ( -5.499998387031001634, -20.49508120620799900, 12.00000000000000000 ) ) ;
#12218 = CARTESIAN_POINT ( 'NONE',  ( 29.34898802046944155, -4.500875419183088866, 7.939653947423662039 ) ) ;
#12219 = CARTESIAN_POINT ( 'NONE',  ( 29.79859849048667897, -1.928627242885762705, 5.783357778048662468 ) ) ;
#12220 = DIRECTION ( 'NONE',  ( 0.000000000000000000, 0.000000000000000000, -1.000000000000000000 ) ) ;
#12221 = CARTESIAN_POINT ( 'NONE',  ( 27.55969062878875064, -7.234529412811931515, -5.783357778048668685 ) ) ;
#12223 = VECTOR ( 'NONE', #1335, 1000.000000000000000 ) ;
#12222 = CARTESIAN_POINT ( 'NONE',  ( 1.296864337298335788E-21, -1.182044466681725685E-21, -6.899999999999998579 ) ) ;
#12224 = CARTESIAN_POINT ( 'NONE',  ( 30.63309003953906995, -6.864245478665264244, 5.783357778048664244 ) ) ;
#12225 = CARTESIAN_POINT ( 'NONE',  ( 31.98525019727866692, -6.363978266284800789, -7.033357778048666908 ) ) ;
#12226 = PLANE ( 'NONE',  #9052 ) ;
#12227 = EDGE_CURVE ( 'NONE', #15184, #17384, #5802, .T. ) ;
#12228 = CARTESIAN_POINT ( 'NONE',  ( 18.06432791129289939, -12.37828432491873443, -15.83774382844986484 ) ) ;
#12229 = CARTESIAN_POINT ( 'NONE',  ( 29.24999999999999645, -15.80522841342829921, 13.37255996287877480 ) ) ;
#12230 = EDGE_CURVE ( 'NONE', #10572, #1595, #2638, .T. ) ;
#12231 = CIRCLE ( 'NONE', #16013, 10.50000000000000000 ) ;
#12232 = AXIS2_PLACEMENT_3D ( 'NONE', #15238, #6992, #16696 ) ;
#12233 =( BOUNDED_CURVE ( )  B_SPLINE_CURVE ( 2, ( #5907, #10343, #2128, #662, #11707, #7650, #6276, #6185, #14547 ),
 .UNSPECIFIED., .F., .F. ) 
 B_SPLINE_CURVE_WITH_KNOTS ( ( 3, 2, 2, 2, 3 ),
 ( 0.7884615384615384359, 0.7948717948717948234, 0.8076923076923077094, 0.8205128205128204844, 0.8269230769230769829 ),
 .UNSPECIFIED. ) 
 CURVE ( )  GEOMETRIC_REPRESENTATION_ITEM ( )  RATIONAL_B_SPLINE_CURVE ( ( 0.9330127018922194093, 0.9330127018922194093, 1.000000000000000000, 0.8660254037844387076, 1.000000000000000000, 0.8660254037844387076, 1.000000000000000000, 0.9330127018922187432, 0.9330127018922192983 ) ) 
 REPRESENTATION_ITEM ( '' )  );
#12234 = CARTESIAN_POINT ( 'NONE',  ( 32.19919549706052209, -6.038393303862174655, -4.705209693361169343 ) ) ;
#12235 = CARTESIAN_POINT ( 'NONE',  ( 29.52399153675929355, -1.971908820246954130, -5.783357778048658915 ) ) ;
#12236 = B_SPLINE_CURVE_WITH_KNOTS ( 'NONE', 3,
 ( #2680, #8208, #3947, #15000 ),
 .UNSPECIFIED., .F., .F.,
 ( 4, 4 ),
 ( 0.004328141481285538092, 0.004974662558709086295 ),
 .UNSPECIFIED. ) ;
#12237 = CARTESIAN_POINT ( 'NONE',  ( 50.00000000000000000, -16.03270077640482683, -5.537981825772250843 ) ) ;
#12238 = DIRECTION ( 'NONE',  ( -0.7999999999999999334, 0.6000000000000000888, 0.000000000000000000 ) ) ;
#12239 = AXIS2_PLACEMENT_3D ( 'NONE', #3057, #1614, #1890 ) ;
#12240 = VERTEX_POINT ( 'NONE', #10597 ) ;
#12241 = ORIENTED_EDGE ( 'NONE', *, *, #6303, .F. ) ;
#12242 = CARTESIAN_POINT ( 'NONE',  ( 33.60446413004628141, -3.988174587000466342, 7.939653947423662039 ) ) ;
#12243 = AXIS2_PLACEMENT_3D ( 'NONE', #13884, #16029, #14661 ) ;
#12244 = TOROIDAL_SURFACE ( 'NONE', #6453, 10.40000000000000036, 0.9000000000000003553 ) ;
#12245 = CARTESIAN_POINT ( 'NONE',  ( 28.97253418081003673, -5.800171738120336151, -7.939653947423662927 ) ) ;
#12246 = CIRCLE ( 'NONE', #4428, 2.749999999999991118 ) ;
#12247 = CARTESIAN_POINT ( 'NONE',  ( 33.50243880635947846, -1.482387629897225390, -5.783357778048663356 ) ) ;
#12248 = CYLINDRICAL_SURFACE ( 'NONE', #42, 2.000000000000001776 ) ;
#12249 = DIRECTION ( 'NONE',  ( 1.000000000000000000, 0.000000000000000000, 0.000000000000000000 ) ) ;
#12250 = CARTESIAN_POINT ( 'NONE',  ( 25.80685721358263152, -3.162108319002908896, 7.047028914770492314 ) ) ;
#12251 = LINE ( 'NONE', #11041, #6424 ) ;
#12252 = EDGE_CURVE ( 'NONE', #1184, #5157, #17154, .T. ) ;
#12253 = CIRCLE ( 'NONE', #4152, 2.749999999999988454 ) ;
#12254 = CARTESIAN_POINT ( 'NONE',  ( 27.18555652250208610, -2.580805812949960920, -7.033357778048658027 ) ) ;
#12255 = EDGE_CURVE ( 'NONE', #10066, #6664, #4078, .T. ) ;
#12256 = CARTESIAN_POINT ( 'NONE',  ( 32.14665875496697822, -6.044722943765660439, -6.861505862736166250 ) ) ;
#12257 = CARTESIAN_POINT ( 'NONE',  ( 27.89480254248674740, -2.495355674045408367, -7.033357778048658027 ) ) ;
#12258 = PLANE ( 'NONE',  #3104 ) ;
#12259 = CARTESIAN_POINT ( 'NONE',  ( 30.37838863598085837, -1.858773980305536089, 6.453230759126469707 ) ) ;
#12260 = DIRECTION ( 'NONE',  ( 0.000000000000000000, 0.000000000000000000, -1.000000000000000000 ) ) ;
#12261 = CARTESIAN_POINT ( 'NONE',  ( 29.64681518302145946, -6.972875258987813574, -5.783357778048668685 ) ) ;
#12262 = EDGE_CURVE ( 'NONE', #17950, #11972, #4097, .T. ) ;
#12263 = B_SPLINE_CURVE_WITH_KNOTS ( 'NONE', 3,
 ( #933, #1026, #6469, #15897, #7911, #4910, #17567, #7730, #13532, #6630, #10438, #9094, #15998, #10608 ),
 .UNSPECIFIED., .F., .F.,
 ( 4, 2, 2, 2, 2, 2, 4 ),
 ( 0.000000000000000000, 0.004968481363098090076, 0.007452722044647132511, 0.009936962726196174947, 0.01490544408929426155, 0.01738968477084330486, 0.01987392545239234642 ),
 .UNSPECIFIED. ) ;
#12264 = CARTESIAN_POINT ( 'NONE',  ( 45.00000000000000711, -19.03270077640482683, 10.53798182577225084 ) ) ;
#12265 = AXIS2_PLACEMENT_3D ( 'NONE', #903, #6525, #5144 ) ;
#12266 = CARTESIAN_POINT ( 'NONE',  ( 3.538288549924106796, -15.34800872113743431, -16.99955934415557479 ) ) ;
#12267 = AXIS2_PLACEMENT_3D ( 'NONE', #4944, #7682, #4850 ) ;
#12268 = EDGE_LOOP ( 'NONE', ( #4994, #1353, #15242, #3054 ) ) ;
#12269 = CARTESIAN_POINT ( 'NONE',  ( 33.95908713831674675, -3.945449517755637903, -5.783357778048663356 ) ) ;
#12270 = CARTESIAN_POINT ( 'NONE',  ( 29.17398450417959310, -7.029842018119214941, -5.783357778048669573 ) ) ;
#12271 = DIRECTION ( 'NONE',  ( 0.9937818688019538493, -0.1113444980252557837, 0.000000000000000000 ) ) ;
#12272 = ORIENTED_EDGE ( 'NONE', *, *, #11121, .T. ) ;
#12273 = EDGE_CURVE ( 'NONE', #2403, #16655, #14880, .T. ) ;
#12274 = CARTESIAN_POINT ( 'NONE',  ( 33.14902674121363901, -1.535163666906202318, -5.783357778048658027 ) ) ;
#12275 = DIRECTION ( 'NONE',  ( 1.000000000000000000, 0.000000000000000000, 0.000000000000000000 ) ) ;
#12276 = DIRECTION ( 'NONE',  ( -0.000000000000000000, -0.000000000000000000, 1.000000000000000000 ) ) ;
#12277 = CARTESIAN_POINT ( 'NONE',  ( 33.69269431359690969, -6.158264969628857166, -4.533357778048668685 ) ) ;
#12278 = ORIENTED_EDGE ( 'NONE', *, *, #13895, .F. ) ;
#12279 = CARTESIAN_POINT ( 'NONE',  ( 28.40369292566375492, -19.36532336263649512, -13.60921607110385523 ) ) ;
#12280 = ORIENTED_EDGE ( 'NONE', *, *, #785, .T. ) ;
#12281 = EDGE_CURVE ( 'NONE', #118, #11675, #17558, .T. ) ;
#12282 = CARTESIAN_POINT ( 'NONE',  ( 29.02054416436834217, -2.659534819136519790, 6.861505862736166250 ) ) ;
#12283 = CARTESIAN_POINT ( 'NONE',  ( 19.43845002722867221, 2.988003976273734263, 0.000000000000000000 ) ) ;
#12284 = CARTESIAN_POINT ( 'NONE',  ( 18.32374253600956493, -20.38504502893476200, 15.79679025666372283 ) ) ;
#12285 = VERTEX_POINT ( 'NONE', #11973 ) ;
#12286 = LINE ( 'NONE', #13646, #1839 ) ;
#12287 = ORIENTED_EDGE ( 'NONE', *, *, #16302, .F. ) ;
#12288 = CARTESIAN_POINT ( 'NONE',  ( 28.01872616749444944, -6.841866079205687790, -4.533357778048668685 ) ) ;
#12289 = ORIENTED_EDGE ( 'NONE', *, *, #6655, .F. ) ;
#12290 = FACE_OUTER_BOUND ( 'NONE', #12406, .T. ) ;
#12291 = CARTESIAN_POINT ( 'NONE',  ( 29.67743187657054449, -6.342216019229654833, -4.705209693361169343 ) ) ;
#12293 = ADVANCED_FACE ( 'NONE', ( #13610 ), #12248, .T. ) ;
#12292 = UNCERTAINTY_MEASURE_WITH_UNIT (LENGTH_MEASURE( 1.000000000000000082E-05 ), #979, 'distance_accuracy_value', 'NONE');
#12294 = CARTESIAN_POINT ( 'NONE',  ( -4.000000000000000000, -0.7890432684750876557, -0.04868663549882429331 ) ) ;
#12295 = CARTESIAN_POINT ( 'NONE',  ( 4.211140560182196957, 2.431303136016537803, -3.445885042887434579 ) ) ;
#12296 = DIRECTION ( 'NONE',  ( 0.000000000000000000, 0.000000000000000000, 1.000000000000000000 ) ) ;
#12297 = CARTESIAN_POINT ( 'NONE',  ( 32.34851646621051202, -1.621412483717243447, 6.453230759126471483 ) ) ;
#12298 = PRODUCT_DEFINITION_SHAPE ( 'NONE', 'NONE',  #15223 ) ;
#12299 = CARTESIAN_POINT ( 'NONE',  ( 27.60205212784272177, -2.830435096530727446, 6.861505862736165362 ) ) ;
#12300 = CARTESIAN_POINT ( 'NONE',  ( 26.01652455409633902, -4.902371455920926380, 5.783357778048663356 ) ) ;
#12301 = LINE ( 'NONE', #2692, #8933 ) ;
#12302 = DIRECTION ( 'NONE',  ( -0.05980762113533058533, 0.4964101615137755386, 0.8660254037844385966 ) ) ;
#12303 = EDGE_LOOP ( 'NONE', ( #13041, #2865, #6429 ) ) ;
#12304 = ORIENTED_EDGE ( 'NONE', *, *, #11893, .F. ) ;
#12305 = ADVANCED_FACE ( 'NONE', ( #8250 ), #2729, .F. ) ;
#12306 = CARTESIAN_POINT ( 'NONE',  ( 30.13703915187255689, -4.405930820630744371, 3.627061608673664228 ) ) ;
#12307 = CARTESIAN_POINT ( 'NONE',  ( 28.67914455963771303, -4.581578327848842669, -8.283357778048662468 ) ) ;
#12308 = EDGE_LOOP ( 'NONE', ( #14157, #3549, #66, #17870 ) ) ;
#12309 = CARTESIAN_POINT ( 'NONE',  ( 30.60986983071443390, -4.348964061499348333, 7.939653947423662039 ) ) ;
#12310 = DIRECTION ( 'NONE',  ( 1.000000000000000000, 0.000000000000000000, 0.000000000000000000 ) ) ;
#12311 = DIRECTION ( 'NONE',  ( -0.000000000000000000, -0.000000000000000000, 1.000000000000000000 ) ) ;
#12312 = PLANE ( 'NONE',  #14230 ) ;
#12313 =( BOUNDED_CURVE ( )  B_SPLINE_CURVE ( 2, ( #2370, #11772, #14516, #3444, #9069, #8974, #4793, #15781, #11959 ),
 .UNSPECIFIED., .F., .T. ) 
 B_SPLINE_CURVE_WITH_KNOTS ( ( 3, 2, 2, 2, 3 ),
 ( 0.7500000000000000000, 0.7564102564102563875, 0.7692307692307692735, 0.7820512820512820484, 0.7884615384615384359 ),
 .UNSPECIFIED. ) 
 CURVE ( )  GEOMETRIC_REPRESENTATION_ITEM ( )  RATIONAL_B_SPLINE_CURVE ( ( 0.9330127018922194093, 0.9330127018922194093, 1.000000000000000000, 0.8660254037844387076, 1.000000000000000000, 0.8660254037844387076, 1.000000000000000000, 0.9330127018922194093, 0.9330127018922194093 ) ) 
 REPRESENTATION_ITEM ( '' )  );
#12314 = CARTESIAN_POINT ( 'NONE',  ( 29.78612525785423060, -2.267488637519798012, -7.033357778048658027 ) ) ;
#12315 = DIRECTION ( 'NONE',  ( -1.000000000000000000, 0.000000000000000000, 0.000000000000000000 ) ) ;
#12316 = EDGE_CURVE ( 'NONE', #8115, #17584, #320, .T. ) ;
#12317 = CARTESIAN_POINT ( 'NONE',  ( 26.79770707206266778, -11.23794579741151090, -14.03572743982056181 ) ) ;
#12318 = DIRECTION ( 'NONE',  ( -0.1196152422706610735, 0.9928203230275511881, 0.000000000000000000 ) ) ;
#12319 = FILL_AREA_STYLE ('',( #6963 ) ) ;
#12320 = CARTESIAN_POINT ( 'NONE',  ( 32.07220196432897552, -5.426722983814484813, -3.627061608673668225 ) ) ;
#12321 = CARTESIAN_POINT ( 'NONE',  ( 28.08810621022444920, -4.652786776866828511, -3.627061608673664672 ) ) ;
#12322 = DIRECTION ( 'NONE',  ( 0.1196152422706621143, -0.9928203230275509661, 0.000000000000000000 ) ) ;
#12323 = CARTESIAN_POINT ( 'NONE',  ( 31.58296173575813981, -1.713646710223874381, -6.453230759126465266 ) ) ;
#12324 = VERTEX_POINT ( 'NONE', #16600 ) ;
#12325 = ORIENTED_EDGE ( 'NONE', *, *, #9739, .T. ) ;
#12326 = EDGE_CURVE ( 'NONE', #9522, #9058, #5516, .T. ) ;
#12327 = CARTESIAN_POINT ( 'NONE',  ( 31.91459173804835103, -5.445711903524953712, 7.939653947423658487 ) ) ;
#12328 = CARTESIAN_POINT ( 'NONE',  ( 29.50659824675005893, -4.481886499472614638, -7.939653947423662039 ) ) ;
#12329 = DIRECTION ( 'NONE',  ( 0.5000000000000014433, 0.8660254037844378194, -0.000000000000000000 ) ) ;
#12330 = DIRECTION ( 'NONE',  ( 0.8243186046180107640, -0.5661261679878571984, -0.000000000000000000 ) ) ;
#12331 = CARTESIAN_POINT ( 'NONE',  ( 28.12741954877813555, -2.767138697495831856, -6.861505862736159145 ) ) ;
#12332 = CARTESIAN_POINT ( 'NONE',  ( 0.000000000000000000, 0.000000000000000000, -2.000000000000000000 ) ) ;
#12333 = FACE_OUTER_BOUND ( 'NONE', #8416, .T. ) ;
#12334 = CARTESIAN_POINT ( 'NONE',  ( 2.500000000000000000, 1.178949249685213863, -2.042000000000001148 ) ) ;
#12335 = ADVANCED_FACE ( 'NONE', ( #1727 ), #5690, .T. ) ;
#12336 = CARTESIAN_POINT ( 'NONE',  ( 28.28511899221430070, -4.629050627332469858, -3.283357778048664688 ) ) ;
#12337 = PRODUCT_DEFINITION ( 'UNKNOWN', '', #11179, #11686 ) ;
#12338 = EDGE_LOOP ( 'NONE', ( #8836, #2723, #14936, #3791 ) ) ;
#12339 = CARTESIAN_POINT ( 'NONE',  ( 33.60446413004628141, -3.988174587000466342, -3.627061608673664672 ) ) ;
#12340 = CARTESIAN_POINT ( 'NONE',  ( 27.17934203385504333, -30.00000000000000355, 12.00000000000000000 ) ) ;
#12341 = CARTESIAN_POINT ( 'NONE',  ( 0.000000000000000000, 0.000000000000000000, 10.50000000000000000 ) ) ;
#12342 = CARTESIAN_POINT ( 'NONE',  ( -45.00000000000000711, -16.03270077640482683, 0.5379818257722508434 ) ) ;
#12343 = CARTESIAN_POINT ( 'NONE',  ( 28.88938074516742205, -6.437160617781993999, -4.705209693361168455 ) ) ;
#12344 = ORIENTED_EDGE ( 'NONE', *, *, #8818, .T. ) ;
#12345 = ADVANCED_FACE ( 'NONE', ( #11035 ), #9857, .F. ) ;
#12346 = EDGE_LOOP ( 'NONE', ( #9514, #11510 ) ) ;
#12347 = CARTESIAN_POINT ( 'NONE',  ( -28.91489957058744409, -14.18850833160549207, -13.46727466850441601 ) ) ;
#12348 = ORIENTED_EDGE ( 'NONE', *, *, #11893, .T. ) ;
#12349 = CARTESIAN_POINT ( 'NONE',  ( 30.92509028327567933, -4.310986222078405206, -7.939653947423662039 ) ) ;
#12350 = DIRECTION ( 'NONE',  ( 0.000000000000000000, 0.000000000000000000, 1.000000000000000000 ) ) ;
#12351 = EDGE_CURVE ( 'NONE', #16041, #11613, #9678, .T. ) ;
#12352 = ORIENTED_EDGE ( 'NONE', *, *, #16158, .F. ) ;
#12353 = CARTESIAN_POINT ( 'NONE',  ( 32.67202617590239555, -5.981426544730773287, -4.705209693361168455 ) ) ;
#12354 = CYLINDRICAL_SURFACE ( 'NONE', #1149, 2.000000000000001776 ) ;
#12355 = CARTESIAN_POINT ( 'NONE',  ( 4.211405962802042602, 2.460462805100870565, -3.451298870276226172 ) ) ;
#12356 = CARTESIAN_POINT ( 'NONE',  ( 28.40332666278570173, -4.614808937445885384, -7.939653947423662039 ) ) ;
#12357 = VERTEX_POINT ( 'NONE', #272 ) ;
#12358 = CARTESIAN_POINT ( 'NONE',  ( 23.43992347230441453, -22.46596520570847844, -14.83047979245100656 ) ) ;
#12359 = ORIENTED_EDGE ( 'NONE', *, *, #14347, .F. ) ;
#12360 = ORIENTED_EDGE ( 'NONE', *, *, #11729, .T. ) ;
#12361 = EDGE_CURVE ( 'NONE', #6537, #7694, #4805, .T. ) ;
#12362 = AXIS2_PLACEMENT_3D ( 'NONE', #17281, #12990, #10075 ) ;
#12363 = B_SPLINE_CURVE_WITH_KNOTS ( 'NONE', 1,
 ( #15585, #7080 ),
 .UNSPECIFIED., .F., .F.,
 ( 2, 2 ),
 ( 0.000000000000000000, 1.000000000000000000 ),
 .UNSPECIFIED. ) ;
#12364 = CARTESIAN_POINT ( 'NONE',  ( 26.62577407660990758, -3.575027854551694695, 7.939653947423664704 ) ) ;
#12365 = CARTESIAN_POINT ( 'NONE',  ( 25.71748644841968456, -2.420320648352046078, 5.783357778048663356 ) ) ;
#12366 = EDGE_LOOP ( 'NONE', ( #6003, #295, #1751, #12908 ) ) ;
#12367 = ORIENTED_EDGE ( 'NONE', *, *, #1138, .F. ) ;
#12368 = CARTESIAN_POINT ( 'NONE',  ( 28.11132641904908169, -7.168068194032743534, -5.783357778048668685 ) ) ;
#12369 = DIRECTION ( 'NONE',  ( 0.1196152422706605323, -0.9928203230275512992, 0.000000000000000000 ) ) ;
#12370 = EDGE_CURVE ( 'NONE', #13758, #15536, #9018, .T. ) ;
#12371 = CARTESIAN_POINT ( 'NONE',  ( 28.30694982360322953, -3.372479377640031473, -7.939653947423660263 ) ) ;
#12372 = CARTESIAN_POINT ( 'NONE',  ( -3.455075492487832634, 2.624013387858676438, -3.016622336521400882 ) ) ;
#12373 = CARTESIAN_POINT ( 'NONE',  ( 28.09001152836988524, -6.106370808549102414, 3.283357778048663356 ) ) ;
#12374 = CARTESIAN_POINT ( 'NONE',  ( 0.000000000000000000, 0.000000000000000000, 0.000000000000000000 ) ) ;
#12375 = CARTESIAN_POINT ( 'NONE',  ( 26.88845778707760914, -3.543379655034240905, 3.627061608673666893 ) ) ;
#12376 = CARTESIAN_POINT ( 'NONE',  ( 30.23341599105502908, -5.648260380436597394, 3.627061608673662896 ) ) ;
#12377 = VECTOR ( 'NONE', #16594, 1000.000000000000227 ) ;
#12378 = CARTESIAN_POINT ( 'NONE',  ( 2.500000000000000000, 2.357898499370432166, -2.385244779468109755E-15 ) ) ;
#12379 = CARTESIAN_POINT ( 'NONE',  ( -7.511572993685817836E-16, -4.618802153517020059, -4.700000000000000178 ) ) ;
#12380 = CYLINDRICAL_SURFACE ( 'NONE', #1487, 2.749999999999992006 ) ;
#12381 = ORIENTED_EDGE ( 'NONE', *, *, #16624, .F. ) ;
#12382 = EDGE_CURVE ( 'NONE', #2104, #16590, #10040, .T. ) ;
#12383 = ORIENTED_EDGE ( 'NONE', *, *, #12039, .F. ) ;
#12384 = CARTESIAN_POINT ( 'NONE',  ( 32.79901970863393501, -6.593096864778464017, 5.783357778048658027 ) ) ;
#12385 = CARTESIAN_POINT ( 'NONE',  ( 36.07773319708005744, -23.32620662758124297, 11.14818368178938357 ) ) ;
#12386 = VERTEX_POINT ( 'NONE', #1549 ) ;
#12387 = CARTESIAN_POINT ( 'NONE',  ( 30.29464937815318493, -4.386941900920275472, 3.627061608673664228 ) ) ;
#12388 = ORIENTED_EDGE ( 'NONE', *, *, #4966, .F. ) ;
#12389 = DIRECTION ( 'NONE',  ( -0.000000000000000000, 1.000000000000000000, -3.469446951953614189E-16 ) ) ;
#12390 = CARTESIAN_POINT ( 'NONE',  ( 27.27683486999669427, -2.232449958253242883, 5.783357778048667797 ) ) ;
#12391 = CARTESIAN_POINT ( 'NONE',  ( 29.35841309260160159, -6.680460261459264970, 7.033357778048657138 ) ) ;
#12392 = CIRCLE ( 'NONE', #15583, 13.00000000000000178 ) ;
#12393 = CARTESIAN_POINT ( 'NONE',  ( 26.31128205117621022, -7.047579375861630524, -7.033357778048666908 ) ) ;
#12394 = DIRECTION ( 'NONE',  ( 1.000000000000000000, 0.000000000000000000, -0.000000000000000000 ) ) ;
#12395 = EDGE_CURVE ( 'NONE', #6479, #2500, #9665, .T. ) ;
#12396 = CARTESIAN_POINT ( 'NONE',  ( 29.75233713454258933, -1.544652646670201523, -5.783357778048658027 ) ) ;
#12397 = DIRECTION ( 'NONE',  ( 0.9928203230275510771, 0.1196152422706609902, 4.006172263299092517E-17 ) ) ;
#12398 = LINE ( 'NONE', #5497, #14467 ) ;
#12399 = CARTESIAN_POINT ( 'NONE',  ( 26.24741491880506672, -3.420740141806666301, 8.283357778048666020 ) ) ;
#12400 = CIRCLE ( 'NONE', #15883, 2.100000000000000089 ) ;
#12401 = EDGE_CURVE ( 'NONE', #10034, #9359, #371, .T. ) ;
#12402 = CARTESIAN_POINT ( 'NONE',  ( 28.41655006632555569, -6.494127376913395366, -4.705209693361169343 ) ) ;
#12403 = CARTESIAN_POINT ( 'NONE',  ( 27.04606801335823718, -3.524390735323771118, -7.939653947423660263 ) ) ;
#12404 = ORIENTED_EDGE ( 'NONE', *, *, #16011, .T. ) ;
#12405 = CARTESIAN_POINT ( 'NONE',  ( 31.90644508241650357, -6.373472726347483963, -7.033357778048666908 ) ) ;
#12406 = EDGE_LOOP ( 'NONE', ( #211, #3622, #433, #14660 ) ) ;
#12407 = ORIENTED_EDGE ( 'NONE', *, *, #11382, .T. ) ;
#12408 = ORIENTED_EDGE ( 'NONE', *, *, #16637, .F. ) ;
#12409 = CARTESIAN_POINT ( 'NONE',  ( 33.19286683830256379, -2.783822866615540459, 3.627061608673666449 ) ) ;
#12410 = CARTESIAN_POINT ( 'NONE',  ( 27.60205212784272177, -2.830435096530727446, -4.705209693361161349 ) ) ;
#12411 =( BOUNDED_CURVE ( )  B_SPLINE_CURVE ( 2, ( #17155, #10311, #15868, #4879, #17341, #6057, #6434, #11861, #3440 ),
 .UNSPECIFIED., .F., .T. ) 
 B_SPLINE_CURVE_WITH_KNOTS ( ( 3, 2, 2, 2, 3 ),
 ( 0.2500000000000000000, 0.2564102564102563875, 0.2692307692307692180, 0.2820512820512820484, 0.2884615384615384914 ),
 .UNSPECIFIED. ) 
 CURVE ( )  GEOMETRIC_REPRESENTATION_ITEM ( )  RATIONAL_B_SPLINE_CURVE ( ( 0.9330127018922194093, 0.9330127018922195203, 1.000000000000000000, 0.8660254037844387076, 1.000000000000000000, 0.8660254037844387076, 1.000000000000000000, 0.9330127018922190762, 0.9330127018922194093 ) ) 
 REPRESENTATION_ITEM ( '' )  );
#12412 = CARTESIAN_POINT ( 'NONE',  ( 38.97925773053390941, -7.992821573592766349, -5.783357778048662468 ) ) ;
#12413 = DIRECTION ( 'NONE',  ( -0.000000000000000000, -0.000000000000000000, 1.000000000000000000 ) ) ;
#12414 = CARTESIAN_POINT ( 'NONE',  ( -1.500000000000000000, -11.00000000000000000, -9.708203932499369415 ) ) ;
#12415 = CARTESIAN_POINT ( 'NONE',  ( 29.41022140756759029, -3.239556939666760726, -7.939653947423660263 ) ) ;
#12416 = CARTESIAN_POINT ( 'NONE',  ( 26.69778786461289855, -6.274106265784127778, -3.283357778048667797 ) ) ;
#12417 = DIRECTION ( 'NONE',  ( -0.000000000000000000, -0.000000000000000000, -1.000000000000000000 ) ) ;
#12418 = AXIS2_PLACEMENT_3D ( 'NONE', #17852, #5372, #7942 ) ;
#12419 = DIRECTION ( 'NONE',  ( 1.000000000000000000, 0.000000000000000000, 0.000000000000000000 ) ) ;
#12420 = CARTESIAN_POINT ( 'NONE',  ( 27.65467808709180630, -4.705006306174339237, -3.283357778048664688 ) ) ;
#12421 = EDGE_CURVE ( 'NONE', #16561, #82, #8519, .T. ) ;
#12422 = CARTESIAN_POINT ( 'NONE',  ( 29.39282811755836633, -5.749534618892433002, -3.627061608673667781 ) ) ;
#12423 = CARTESIAN_POINT ( 'NONE',  ( 33.95908713831673964, -3.945449517755637014, 5.783357778048663356 ) ) ;
#12424 = CARTESIAN_POINT ( 'NONE',  ( 26.01652455409633902, -4.902371455920928156, -5.783357778048663356 ) ) ;
#12425 = CARTESIAN_POINT ( 'NONE',  ( 19.43845002722867221, 2.988003976273734263, 6.000000000000000000 ) ) ;
#12426 = AXIS2_PLACEMENT_3D ( 'NONE', #9723, #11452, #17019 ) ;
#12427 = CARTESIAN_POINT ( 'NONE',  ( -4.175003227304314279, -2.208362916365308681, -3.169254239516212657 ) ) ;
#12428 = CARTESIAN_POINT ( 'NONE',  ( 28.77978050244509944, -3.315512618508630549, -7.939653947423660263 ) ) ;
#12429 = AXIS2_PLACEMENT_3D ( 'NONE', #13840, #11181, #1262 ) ;
#12430 = EDGE_CURVE ( 'NONE', #9791, #2920, #2292, .T. ) ;
#12431 = VERTEX_POINT ( 'NONE', #1361 ) ;
#12432 = ORIENTED_EDGE ( 'NONE', *, *, #14879, .F. ) ;
#12433 = ORIENTED_EDGE ( 'NONE', *, *, #2769, .F. ) ;
#12434 = DIRECTION ( 'NONE',  ( 0.000000000000000000, 0.000000000000000000, 1.000000000000000000 ) ) ;
#12435 = CARTESIAN_POINT ( 'NONE',  ( 34.91600907648203389, -11.88801210197604341, -11.56671555609732671 ) ) ;
#12436 = DIRECTION ( 'NONE',  ( -0.000000000000000000, -0.000000000000000000, -1.000000000000000000 ) ) ;
#12437 = EDGE_LOOP ( 'NONE', ( #5572, #8902 ) ) ;
#12438 = PRODUCT_DEFINITION_SHAPE ( 'NONE', 'NONE',  #17982 ) ;
#12439 = CARTESIAN_POINT ( 'NONE',  ( 29.78250536075762867, -6.329556739422670830, -6.861505862736167138 ) ) ;
#12440 = CARTESIAN_POINT ( 'NONE',  ( 28.82057243903374655, -7.082618055128190093, -5.783357778048668685 ) ) ;
#12441 = UNCERTAINTY_MEASURE_WITH_UNIT (LENGTH_MEASURE( 1.000000000000000082E-05 ), #17825, 'distance_accuracy_value', 'NONE');
#12442 = AXIS2_PLACEMENT_3D ( 'NONE', #15539, #3122, #7214 ) ;
#12443 = EDGE_CURVE ( 'NONE', #7377, #3411, #11053, .T. ) ;
#12444 = CARTESIAN_POINT ( 'NONE',  ( 27.32822876973539294, -6.198150586942257512, -3.283357778048667797 ) ) ;
#12445 = ADVANCED_FACE ( 'NONE', ( #2186 ), #540, .T. ) ;
#12446 = CARTESIAN_POINT ( 'NONE',  ( 29.62480591732145996, -4.467644809586046151, 8.283357778048662468 ) ) ;
#12447 = DIRECTION ( 'NONE',  ( 0.000000000000000000, 0.000000000000000000, -1.000000000000000000 ) ) ;
#12448 = CARTESIAN_POINT ( 'NONE',  ( 26.82722439997946395, -4.804698134550569044, -3.627061608673664672 ) ) ;
#12449 = DIRECTION ( 'NONE',  ( -1.000000000000000000, 0.000000000000000000, 0.000000000000000000 ) ) ;
#12450 = VERTEX_POINT ( 'NONE', #7436 ) ;
#12451 = AXIS2_PLACEMENT_3D ( 'NONE', #3128, #11255, #16833 ) ;
#12452 = CIRCLE ( 'NONE', #15065, 13.00000000000000178 ) ;
#12453 = MECHANICAL_DESIGN_GEOMETRIC_PRESENTATION_REPRESENTATION (  '', ( #10134 ), #6959 ) ;
#12454 = CARTESIAN_POINT ( 'NONE',  ( 25.78518620311324838, -3.676302093007511651, 3.627061608673666893 ) ) ;
#12455 =( NAMED_UNIT ( * ) PLANE_ANGLE_UNIT ( ) SI_UNIT ( $, .RADIAN. ) );
#12456 = LINE ( 'NONE', #4028, #16209 ) ;
#12457 = ORIENTED_EDGE ( 'NONE', *, *, #6806, .F. ) ;
#12458 = CARTESIAN_POINT ( 'NONE',  ( -45.00000000000000711, -16.03270077640482683, 5.537981825772250843 ) ) ;
#12459 = ORIENTED_EDGE ( 'NONE', *, *, #14498, .F. ) ;
#12460 = DIRECTION ( 'NONE',  ( 0.000000000000000000, 0.000000000000000000, 1.000000000000000000 ) ) ;
#12461 = CIRCLE ( 'NONE', #8395, 2.749999999999988454 ) ;
#12462 = CARTESIAN_POINT ( 'NONE',  ( 29.56783163384821833, -3.220568019956291383, -7.939653947423660263 ) ) ;
#12463 = PRODUCT_DEFINITION_CONTEXT ( 'detailed design', #4811, 'design' ) ;
#12464 = DIRECTION ( 'NONE',  ( 0.9928203230275512992, 0.1196152422706610319, 9.614813431917826478E-17 ) ) ;
#12465 = CARTESIAN_POINT ( 'NONE',  ( 27.84978555093622177, -3.227686124957687586, 3.283357778048666464 ) ) ;
#12466 = DIRECTION ( 'NONE',  ( 0.000000000000000000, 0.000000000000000000, -1.000000000000000000 ) ) ;
#12467 = CARTESIAN_POINT ( 'NONE',  ( 30.78070346053490880, -6.209293581256383199, 6.861505862736158257 ) ) ;
#12468 = AXIS2_PLACEMENT_3D ( 'NONE', #11207, #8334, #183 ) ;
#12469 = ADVANCED_FACE ( 'NONE', ( #11859 ), #8799, .F. ) ;
#12470 = PRESENTATION_LAYER_ASSIGNMENT (  '', '', ( #4649 ) ) ;
#12471 = CARTESIAN_POINT ( 'NONE',  ( -4.000000000000000000, -2.309401076758508253, -3.133295621305383083 ) ) ;
#12472 = DIRECTION ( 'NONE',  ( 0.000000000000000000, 0.000000000000000000, 1.000000000000000000 ) ) ;
#12473 = CARTESIAN_POINT ( 'NONE',  ( -8.776279441628885181, -6.799038105676576293, -2.000000000000000000 ) ) ;
#12474 = ORIENTED_EDGE ( 'NONE', *, *, #5286, .F. ) ;
#12475 = EDGE_CURVE ( 'NONE', #4593, #16631, #11301, .T. ) ;
#12476 = CIRCLE ( 'NONE', #1779, 2.749999999999988454 ) ;
#12477 = ORIENTED_EDGE ( 'NONE', *, *, #11072, .T. ) ;
#12478 = CARTESIAN_POINT ( 'NONE',  ( 28.10549950023366961, -2.142809097641162897, 5.783357778048668685 ) ) ;
#12479 = DIRECTION ( 'NONE',  ( -0.4999999999999981126, 0.8660254037844397068, 0.000000000000000000 ) ) ;
#12480 = ORIENTED_EDGE ( 'NONE', *, *, #16289, .F. ) ;
#12481 = CARTESIAN_POINT ( 'NONE',  ( 27.15566825608056689, -6.646038734597135011, 6.861505862736157368 ) ) ;
#12482 = CARTESIAN_POINT ( 'NONE',  ( 32.95080301609915097, -1.548848848676412260, -5.783357778048663356 ) ) ;
#12483 = VECTOR ( 'NONE', #3708, 1000.000000000000114 ) ;
#12484 = DIRECTION ( 'NONE',  ( 0.000000000000000000, 0.000000000000000000, -1.000000000000000000 ) ) ;
#12485 = CARTESIAN_POINT ( 'NONE',  ( 8.472608240843633681E-22, -7.722472891792491889E-22, -7.794427190999915211 ) ) ;
#12486 = CARTESIAN_POINT ( 'NONE',  ( 27.14244485254070938, -4.766720295129625029, -7.939653947423662039 ) ) ;
#12487 = CARTESIAN_POINT ( 'NONE',  ( 0.000000000000000000, 0.000000000000000000, 1.599999999999998979 ) ) ;
#12488 = ORIENTED_EDGE ( 'NONE', *, *, #3587, .F. ) ;
#12489 = CARTESIAN_POINT ( 'NONE',  ( 29.26075783691881682, -2.330785036554694489, -4.533357778048659803 ) ) ;
#12490 = DIRECTION ( 'NONE',  ( 0.9928203230275512992, 0.1196152422706614898, -0.000000000000000000 ) ) ;
#12491 = CARTESIAN_POINT ( 'NONE',  ( 21.62432203902686823, -10.11801842300244125, -15.20615207729255403 ) ) ;
#12492 = DIRECTION ( 'NONE',  ( -0.000000000000000000, -0.000000000000000000, -1.000000000000000000 ) ) ;
#12493 =( NAMED_UNIT ( * ) SI_UNIT ( $, .STERADIAN. ) SOLID_ANGLE_UNIT ( ) );
#12494 = CARTESIAN_POINT ( 'NONE',  ( 30.23341599105502908, -5.648260380436597394, -7.939653947423664704 ) ) ;
#12495 = ORIENTED_EDGE ( 'NONE', *, *, #6450, .T. ) ;
#12496 = COLOUR_RGB ( '', 0.31764706, 0.68627451, 0.89019608) ;
#12497 = ADVANCED_FACE ( 'NONE', ( #3438, #15776 ), #3350, .F. ) ;
#12498 = CARTESIAN_POINT ( 'NONE',  ( 30.17635249042624679, -2.520282741259753045, -6.861505862736158257 ) ) ;
#12499 = CYLINDRICAL_SURFACE ( 'NONE', #13860, 95.00000000000000000 ) ;
#12500 = VECTOR ( 'NONE', #8076, 1000.000000000000114 ) ;
#12501 = ORIENTED_EDGE ( 'NONE', *, *, #2485, .F. ) ;
#12502 = EDGE_CURVE ( 'NONE', #8079, #15284, #11955, .T. ) ;
#12503 = ORIENTED_EDGE ( 'NONE', *, *, #8089, .T. ) ;
#12504 = ORIENTED_EDGE ( 'NONE', *, *, #12167, .F. ) ;
#12505 = CARTESIAN_POINT ( 'NONE',  ( 27.71165237056504793, -5.952083095804076684, 3.627061608673662896 ) ) ;
#12506 = CARTESIAN_POINT ( 'NONE',  ( 25.90934487712385348, 0.1208734971681838660, 5.783357778048663356 ) ) ;
#12507 = CARTESIAN_POINT ( 'NONE',  ( 9.749999999999982236, -3.897114317030018871, -3.000000000000000000 ) ) ;
#12508 = LINE ( 'NONE', #9677, #8672 ) ;
#12509 = DIRECTION ( 'NONE',  ( 1.000000000000000000, 1.224646799147353207E-16, 0.000000000000000000 ) ) ;
#12510 = CARTESIAN_POINT ( 'NONE',  ( 30.27725608814395031, -6.896919580145944195, -5.783357778048668685 ) ) ;
#12511 = DIRECTION ( 'NONE',  ( -1.000000000000000000, 0.000000000000000000, 0.000000000000000000 ) ) ;
#12512 = FACE_OUTER_BOUND ( 'NONE', #4074, .T. ) ;
#12513 = VECTOR ( 'NONE', #12109, 1000.000000000000000 ) ;
#12514 = AXIS2_PLACEMENT_3D ( 'NONE', #3892, #7974, #12315 ) ;
#12515 = LINE ( 'NONE', #16430, #642 ) ;
#12516 = CARTESIAN_POINT ( 'NONE',  ( 29.14074637024071635, -5.979778010479330774, -3.283357778048667797 ) ) ;
#12517 = ADVANCED_FACE ( 'NONE', ( #12128 ), #15027, .F. ) ;
#12518 = CARTESIAN_POINT ( 'NONE',  ( 31.25770402584614516, -1.763030703431812674, -5.783357778048658027 ) ) ;
#12519 = DIRECTION ( 'NONE',  ( 0.000000000000000000, -1.224646799147353454E-16, 1.000000000000000000 ) ) ;
#12520 = DIRECTION ( 'NONE',  ( 0.9928203230275512992, 0.1196152422706614898, -0.000000000000000000 ) ) ;
#12521 = CARTESIAN_POINT ( 'NONE',  ( 26.75784435724945709, -6.993777436889428323, 7.033357778048657138 ) ) ;
#12522 = CARTESIAN_POINT ( 'NONE',  ( 30.30397292480292037, -1.478191427891014431, 5.783357778048668685 ) ) ;
#12523 = CARTESIAN_POINT ( 'NONE',  ( 26.97161122272022382, -2.906390775372597712, -4.705209693361161349 ) ) ;
#12524 = ORIENTED_EDGE ( 'NONE', *, *, #8996, .T. ) ;
#12525 = DIRECTION ( 'NONE',  ( 0.9928203230275512992, 0.1196152422706610180, 4.006172263299093133E-17 ) ) ;
#12526 = CARTESIAN_POINT ( 'NONE',  ( 29.95125523467787332, -2.974500528818129652, -3.283357778048662023 ) ) ;
#12527 = EDGE_CURVE ( 'NONE', #14539, #5005, #9769, .T. ) ;
#12528 = ORIENTED_EDGE ( 'NONE', *, *, #3564, .F. ) ;
#12529 = CARTESIAN_POINT ( 'NONE',  ( -17.60362937644963921, -13.05831870693043584, -15.90927928682413928 ) ) ;
#12530 = AXIS2_PLACEMENT_3D ( 'NONE', #3329, #16847, #14113 ) ;
#12531 = VERTEX_POINT ( 'NONE', #13502 ) ;
#12532 = CARTESIAN_POINT ( 'NONE',  ( 28.39010325924584421, -2.735490497978389612, -4.705209693361160461 ) ) ;
#12533 = CARTESIAN_POINT ( 'NONE',  ( 0.000000000000000000, 0.000000000000000000, -8.722503561260788629 ) ) ;
#12534 = VERTEX_POINT ( 'NONE', #6432 ) ;
#12535 = VERTEX_POINT ( 'NONE', #14945 ) ;
#12536 = CARTESIAN_POINT ( 'NONE',  ( 31.88814493096863956, -1.687075024589942851, -5.783357778048658027 ) ) ;
#12537 = EDGE_CURVE ( 'NONE', #3273, #16640, #1695, .T. ) ;
#12538 = CARTESIAN_POINT ( 'NONE',  ( -5.816800114226745675E-16, -4.862606272033100474, -3.445885042887441241 ) ) ;
#12539 = FACE_OUTER_BOUND ( 'NONE', #17241, .T. ) ;
#12540 = CARTESIAN_POINT ( 'NONE',  ( 31.80137159822941939, -6.386132006154467078, -4.533357778048668685 ) ) ;
#12541 = CARTESIAN_POINT ( 'NONE',  ( -13.00000000000000178, -1.592040838891559293E-15, 12.00000000000000000 ) ) ;
#12542 = CIRCLE ( 'NONE', #100, 0.5155456020628804703 ) ;
#12543 = VERTEX_POINT ( 'NONE', #17797 ) ;
#12544 = CARTESIAN_POINT ( 'NONE',  ( 27.92859066579839222, -3.218191664895003967, 3.283357778048666464 ) ) ;
#12545 = EDGE_CURVE ( 'NONE', #10545, #1595, #3706, .T. ) ;
#12546 = CARTESIAN_POINT ( 'NONE',  ( 25.99533317148741318, -3.650983533393564517, 7.939653947423664704 ) ) ;
#12547 = CARTESIAN_POINT ( 'NONE',  ( -27.11285657029384666, -20.94160726625447211, 13.95434672273383114 ) ) ;
#12548 = CARTESIAN_POINT ( 'NONE',  ( 25.71748644841968456, -2.420320648352051851, -5.783357778048663356 ) ) ;
#12549 = VERTEX_POINT ( 'NONE', #16326 ) ;
#12550 =( LENGTH_UNIT ( ) NAMED_UNIT ( * ) SI_UNIT ( .MILLI., .METRE. ) );
#12551 = ORIENTED_EDGE ( 'NONE', *, *, #11842, .T. ) ;
#12552 = FACE_OUTER_BOUND ( 'NONE', #15903, .T. ) ;
#12553 = PLANE ( 'NONE',  #14267 ) ;
#12554 = CARTESIAN_POINT ( 'NONE',  ( 27.14244485254070938, -4.766720295129625029, -7.939653947423662039 ) ) ;
#12555 = CARTESIAN_POINT ( 'NONE',  ( 31.29094215978502547, -2.813094711071706389, -3.283357778048662023 ) ) ;
#12556 = VECTOR ( 'NONE', #3331, 1000.000000000000000 ) ;
#12557 = DIRECTION ( 'NONE',  ( 1.000000000000000000, 0.000000000000000000, 0.000000000000000000 ) ) ;
#12558 = EDGE_CURVE ( 'NONE', #17384, #3640, #5539, .T. ) ;
#12559 = PRODUCT_CONTEXT ( 'NONE', #10804, 'mechanical' ) ;
#12560 = DIRECTION ( 'NONE',  ( 0.000000000000000000, 1.000000000000000000, 0.000000000000000000 ) ) ;
#12561 = CARTESIAN_POINT ( 'NONE',  ( 30.13703915187255689, -4.405930820630744371, 3.627061608673664228 ) ) ;
#12562 = LINE ( 'NONE', #57, #8183 ) ;
#12563 = CARTESIAN_POINT ( 'NONE',  ( 32.52441275490655670, -6.636378442139655220, 5.783357778048664244 ) ) ;
#12564 = CARTESIAN_POINT ( 'NONE',  ( 29.67743187657054449, -6.342216019229654833, 6.861505862736157368 ) ) ;
#12565 = ORIENTED_EDGE ( 'NONE', *, *, #10949, .T. ) ;
#12566 = VERTEX_POINT ( 'NONE', #997 ) ;
#12567 = CARTESIAN_POINT ( 'NONE',  ( 28.14933959732260149, -3.391468297350501260, 3.627061608673666893 ) ) ;
#12568 = DIRECTION ( 'NONE',  ( 0.9928203230275512992, 0.1196152422706610180, 4.006172263299093133E-17 ) ) ;
#12569 = CYLINDRICAL_SURFACE ( 'NONE', #12239, 5.000000000000000000 ) ;
#12570 = ORIENTED_EDGE ( 'NONE', *, *, #10531, .F. ) ;
#12571 = CARTESIAN_POINT ( 'NONE',  ( 27.65911562847151117, -5.958412735707574015, 7.939653947423658487 ) ) ;
#12572 = ORIENTED_EDGE ( 'NONE', *, *, #6411, .T. ) ;
#12573 = AXIS2_PLACEMENT_3D ( 'NONE', #15463, #5927, #1601 ) ;
#12574 = ORIENTED_EDGE ( 'NONE', *, *, #14226, .T. ) ;
#12575 =( BOUNDED_CURVE ( )  B_SPLINE_CURVE ( 2, ( #12390, #17958, #5490, #17033, #3332, #3147, #12659, #14117, #5944 ),
 .UNSPECIFIED., .F., .T. ) 
 B_SPLINE_CURVE_WITH_KNOTS ( ( 3, 2, 2, 2, 3 ),
 ( 0.7115384615384615641, 0.7179487179487179516, 0.7307692307692307265, 0.7435897435897436125, 0.7500000000000000000 ),
 .UNSPECIFIED. ) 
 CURVE ( )  GEOMETRIC_REPRESENTATION_ITEM ( )  RATIONAL_B_SPLINE_CURVE ( ( 0.9330127018922194093, 0.9330127018922194093, 1.000000000000000000, 0.8660254037844387076, 1.000000000000000000, 0.8660254037844387076, 1.000000000000000000, 0.9330127018922194093, 0.9330127018922194093 ) ) 
 REPRESENTATION_ITEM ( '' )  );
#12576 = PLANE ( 'NONE',  #7207 ) ;
#12577 = LINE ( 'NONE', #16753, #276 ) ;
#12578 = CARTESIAN_POINT ( 'NONE',  ( 33.50243880635947846, -1.482387629897225390, -5.783357778048663356 ) ) ;
#12579 = CARTESIAN_POINT ( 'NONE',  ( 25.93489015466116854, -5.606035894254070229, -7.939653947423662927 ) ) ;
#12580 = APPLICATION_CONTEXT ( 'automotive_design' ) ;
#12581 = CARTESIAN_POINT ( 'NONE',  ( 33.53059316159333036, -1.478995586096186532, -5.113484796970854340 ) ) ;
#12582 = ORIENTED_EDGE ( 'NONE', *, *, #5265, .T. ) ;
#12583 = CARTESIAN_POINT ( 'NONE',  ( 27.86101441917510257, -1.772519683195811657, -5.783357778048658027 ) ) ;
#12584 = CARTESIAN_POINT ( 'NONE',  ( 17.93919565825226670, -12.54482367096064621, -15.85739159820981747 ) ) ;
#12585 = CARTESIAN_POINT ( 'NONE',  ( 26.92924972366625980, -7.310485091653801781, 5.783357778048669573 ) ) ;
#12586 = EDGE_CURVE ( 'NONE', #16822, #15540, #15702, .T. ) ;
#12587 = CARTESIAN_POINT ( 'NONE',  ( 31.38469755857769528, -2.374701023479507178, -4.705209693361161349 ) ) ;
#12588 = ORIENTED_EDGE ( 'NONE', *, *, #10556, .F. ) ;
#12589 = CARTESIAN_POINT ( 'NONE',  ( 30.43486631442457835, -6.877930660435475296, -5.783357778048669573 ) ) ;
#12590 = DIRECTION ( 'NONE',  ( -0.000000000000000000, -0.000000000000000000, 1.000000000000000000 ) ) ;
#12591 = ORIENTED_EDGE ( 'NONE', *, *, #1996, .F. ) ;
#12592 = ORIENTED_EDGE ( 'NONE', *, *, #6791, .T. ) ;
#12593 = ORIENTED_EDGE ( 'NONE', *, *, #6618, .T. ) ;
#12594 = CARTESIAN_POINT ( 'NONE',  ( 27.09860475545177039, -3.518061095420291995, 7.939653947423662927 ) ) ;
#12595 = CARTESIAN_POINT ( 'NONE',  ( 29.37220822929407760, -7.016156836349003001, -5.783357778048668685 ) ) ;
#12596 = DIRECTION ( 'NONE',  ( -1.000000000000000000, 0.000000000000000000, 0.000000000000000000 ) ) ;
#12597 = EDGE_CURVE ( 'NONE', #14976, #6794, #16406, .T. ) ;
#12598 = SHAPE_REPRESENTATION ( 'heat isolation block', ( #3575 ), #15 ) ;
#12599 = CARTESIAN_POINT ( 'NONE',  ( 32.32036211097666012, -1.624804527518282748, -5.783357778048663356 ) ) ;
#12600 = DIRECTION ( 'NONE',  ( -1.000000000000000000, 0.000000000000000000, 0.000000000000000000 ) ) ;
#12601 = CARTESIAN_POINT ( 'NONE',  ( 30.86385689617752348, -5.572304701594726239, -7.939653947423664704 ) ) ;
#12602 = CARTESIAN_POINT ( 'NONE',  ( 31.94462260941237020, -6.706231704719880504, -5.113484796970860558 ) ) ;
#12603 = CARTESIAN_POINT ( 'NONE',  ( 39.40660799972354056, -7.359808871700536770, -5.783357778048663356 ) ) ;
#12604 = DIRECTION ( 'NONE',  ( -1.000000000000000000, 0.000000000000000000, 0.000000000000000000 ) ) ;
#12605 = UNCERTAINTY_MEASURE_WITH_UNIT (LENGTH_MEASURE( 1.000000000000000082E-05 ), #13555, 'distance_accuracy_value', 'NONE');
#12606 = CARTESIAN_POINT ( 'NONE',  ( 27.49335874655903567, -6.905162478240574053, -7.033357778048666908 ) ) ;
#12607 = ORIENTED_EDGE ( 'NONE', *, *, #12629, .F. ) ;
#12608 = CARTESIAN_POINT ( 'NONE',  ( 30.78070346053490880, -6.209293581256383199, -4.705209693361168455 ) ) ;
#12609 = SURFACE_SIDE_STYLE ('',( #15061 ) ) ;
#12610 = CARTESIAN_POINT ( 'NONE',  ( 2.500000000000000000, 1.178949249685218081, 2.041999999999998483 ) ) ;
#12611 = DIRECTION ( 'NONE',  ( -5.026720092345836698E-22, 4.581671729415424240E-22, -1.000000000000000000 ) ) ;
#12612 = CARTESIAN_POINT ( 'NONE',  ( -1.499999999999999334, 5.809475019311126864, -2.000000000000000000 ) ) ;
#12613 = CARTESIAN_POINT ( 'NONE',  ( 33.10345976029034176, -2.594722134608779207, 8.283357778048664244 ) ) ;
#12614 = CARTESIAN_POINT ( 'NONE',  ( 30.04066231269008469, -3.163601260824890904, -7.939653947423660263 ) ) ;
#12615 = ORIENTED_EDGE ( 'NONE', *, *, #7915, .T. ) ;
#12616 = DIRECTION ( 'NONE',  ( 0.9928203230275510771, 0.1196152422706614621, -0.000000000000000000 ) ) ;
#12617 = DIRECTION ( 'NONE',  ( 0.000000000000000000, 0.000000000000000000, 1.000000000000000000 ) ) ;
#12618 = EDGE_CURVE ( 'NONE', #7363, #8657, #2272, .T. ) ;
#12619 = CARTESIAN_POINT ( 'NONE',  ( 0.2500000000000002220, 0.000000000000000000, 4.000000000000000000 ) ) ;
#12620 = ORIENTED_EDGE ( 'NONE', *, *, #443, .T. ) ;
#12621 = CARTESIAN_POINT ( 'NONE',  ( 26.62577407660990758, -3.575027854551694695, -3.627061608673662008 ) ) ;
#12622 = CARTESIAN_POINT ( 'NONE',  ( 6.540214080563054644, 17.14393242671841477, 16.94648454462088694 ) ) ;
#12623 = ADVANCED_FACE ( 'NONE', ( #14859, #3973 ), #9488, .F. ) ;
#12624 = EDGE_LOOP ( 'NONE', ( #344, #2579, #2428, #1405, #16295 ) ) ;
#12625 = CARTESIAN_POINT ( 'NONE',  ( 29.62036837594175154, -3.214238380052812261, -3.627061608673662896 ) ) ;
#12626 = DIRECTION ( 'NONE',  ( 1.000000000000000000, 0.000000000000000000, 0.000000000000000000 ) ) ;
#12627 = CARTESIAN_POINT ( 'NONE',  ( 4.000000000000000000, 2.512222795755930438, -3.169391084040452000 ) ) ;
#12628 = CARTESIAN_POINT ( 'NONE',  ( 31.00199007654869732, -2.847907730748336252, -8.283357778048658915 ) ) ;
#12629 = EDGE_CURVE ( 'NONE', #10810, #8875, #9586, .T. ) ;
#12630 = CARTESIAN_POINT ( 'NONE',  ( 28.45891156537951971, -2.090033060632186412, 5.783357778048657138 ) ) ;
#12631 = CARTESIAN_POINT ( 'NONE',  ( 31.91006497951310550, -2.311404624444611589, 4.705209693361167567 ) ) ;
#12632 = CARTESIAN_POINT ( 'NONE',  ( 46.86575133767495061, -2.390451368237048069, -5.783357778048661579 ) ) ;
#12633 = FILL_AREA_STYLE_COLOUR ( '', #6082 ) ;
#12634 = CARTESIAN_POINT ( 'NONE',  ( 32.93832978346670615, -1.887710243310447567, 4.533357778048667797 ) ) ;
#12635 = EDGE_LOOP ( 'NONE', ( #7708, #15339, #16767, #5378 ) ) ;
#12636 = VERTEX_POINT ( 'NONE', #7970 ) ;
#12637 = DIRECTION ( 'NONE',  ( 0.000000000000000000, 0.000000000000000000, -1.000000000000000000 ) ) ;
#12638 = ORIENTED_EDGE ( 'NONE', *, *, #10213, .F. ) ;
#12639 = CYLINDRICAL_SURFACE ( 'NONE', #14282, 2.749999999999992006 ) ;
#12640 = CARTESIAN_POINT ( 'NONE',  ( 25.86833963875586306, -3.039313213345869791, -4.705209693361160461 ) ) ;
#12641 = CARTESIAN_POINT ( 'NONE',  ( 33.04340326765378677, -1.875050963503474222, -4.533357778048659803 ) ) ;
#12642 = CARTESIAN_POINT ( 'NONE',  ( 2.500000000000000000, 2.357898499370432166, -2.385244779468109755E-15 ) ) ;
#12643 = APPLICATION_PROTOCOL_DEFINITION ( 'draft international standard', 'automotive_design', 1998, #13620 ) ;
#12644 = CARTESIAN_POINT ( 'NONE',  ( 33.64386668575551198, -3.983427357176565486, 3.283357778048664244 ) ) ;
#12645 = CARTESIAN_POINT ( 'NONE',  ( -4.197393957002304887, -7.639915766855272736E-14, -3.203767560748932208 ) ) ;
#12646 = EDGE_CURVE ( 'NONE', #3121, #16638, #1075, .T. ) ;
#12647 = DIRECTION ( 'NONE',  ( -1.000000000000000000, 0.000000000000000000, 0.000000000000000000 ) ) ;
#12648 = CARTESIAN_POINT ( 'NONE',  ( -11.38175538881593774, -22.33742387525457573, -16.67884400577319681 ) ) ;
#12649 = CARTESIAN_POINT ( 'NONE',  ( 31.65190802758064592, -5.477360103042387074, 3.627061608673662896 ) ) ;
#12650 = VERTEX_POINT ( 'NONE', #9656 ) ;
#12651 = ORIENTED_EDGE ( 'NONE', *, *, #7392, .T. ) ;
#12652 = EDGE_CURVE ( 'NONE', #6066, #16345, #11632, .T. ) ;
#12653 = CARTESIAN_POINT ( 'NONE',  ( 28.76238721243587193, -5.825490297734302381, 7.939653947423658487 ) ) ;
#12654 = CARTESIAN_POINT ( 'NONE',  ( 31.68992120585416217, -1.700760206360153015, -5.783357778048664244 ) ) ;
#12655 = ADVANCED_FACE ( 'NONE', ( #15207 ), #2975, .F. ) ;
#12656 = ORIENTED_EDGE ( 'NONE', *, *, #5702, .T. ) ;
#12657 = CARTESIAN_POINT ( 'NONE',  ( 27.02867472334902033, -6.034368414549445170, 7.939653947423658487 ) ) ;
#12658 = CARTESIAN_POINT ( 'NONE',  ( 8.776279441628796363, -6.799038105676699750, -11.72793873352923910 ) ) ;
#12659 = CARTESIAN_POINT ( 'NONE',  ( 27.57216386142120257, -6.895668018177890879, 4.533357778048659803 ) ) ;
#12660 = CARTESIAN_POINT ( 'NONE',  ( 28.99436501219896201, -4.543600488427916417, 8.283357778048662468 ) ) ;
#12661 = CARTESIAN_POINT ( 'NONE',  ( 0.6920835326022570788, 4.454600218803882683, -3.297382984111581816 ) ) ;
#12662 = CARTESIAN_POINT ( 'NONE',  ( 4.000000000000000888, 1.539600717838997435, -3.000726591567082213 ) ) ;
#12663 = CARTESIAN_POINT ( 'NONE',  ( 28.36392410707646761, -4.619556167269785796, -3.283357778048664688 ) ) ;
#12664 = VECTOR ( 'NONE', #14327, 1000.000000000000227 ) ;
#12665 = LINE ( 'NONE', #12758, #4023 ) ;
#12666 = DIRECTION ( 'NONE',  ( 0.000000000000000000, 0.000000000000000000, -1.000000000000000000 ) ) ;
#12667 = CARTESIAN_POINT ( 'NONE',  ( 31.27962407439061110, -2.387360303286481855, -6.861505862736159145 ) ) ;
#12668 = ORIENTED_EDGE ( 'NONE', *, *, #10886, .T. ) ;
#12669 = EDGE_CURVE ( 'NONE', #558, #6324, #17752, .T. ) ;
#12670 = CARTESIAN_POINT ( 'NONE',  ( 27.28266178881210280, -7.257709054644825741, -5.783357778048669573 ) ) ;
#12671 = DIRECTION ( 'NONE',  ( -0.000000000000000000, -0.000000000000000000, -1.000000000000000000 ) ) ;
#12672 = ORIENTED_EDGE ( 'NONE', *, *, #4516, .T. ) ;
#12673 =( BOUNDED_CURVE ( )  B_SPLINE_CURVE ( 2, ( #4513, #7345, #5951, #11477, #1903, #7427, #14600, #17237, #3695 ),
 .UNSPECIFIED., .F., .T. ) 
 B_SPLINE_CURVE_WITH_KNOTS ( ( 3, 2, 2, 2, 3 ),
 ( 0.5961538461538461453, 0.6025641025641025328, 0.6153846153846154188, 0.6282051282051281937, 0.6346153846153846922 ),
 .UNSPECIFIED. ) 
 CURVE ( )  GEOMETRIC_REPRESENTATION_ITEM ( )  RATIONAL_B_SPLINE_CURVE ( ( 0.9330127018922194093, 0.9330127018922194093, 1.000000000000000000, 0.8660254037844387076, 1.000000000000000000, 0.8660254037844387076, 1.000000000000000000, 0.9330127018922187432, 0.9330127018922192983 ) ) 
 REPRESENTATION_ITEM ( '' )  );
#12674 = CIRCLE ( 'NONE', #6596, 4.250000000000000000 ) ;
#12675 = ORIENTED_EDGE ( 'NONE', *, *, #8861, .F. ) ;
#12676 = CARTESIAN_POINT ( 'NONE',  ( 29.60297508593253468, -5.724216059278466773, 3.627061608673662896 ) ) ;
#12677 = APPLICATION_CONTEXT ( 'automotive_design' ) ;
#12678 = CARTESIAN_POINT ( 'NONE',  ( 31.86581749455020329, -6.715726164782562790, 6.453230759126467042 ) ) ;
#12679 = LINE ( 'NONE', #2996, #3720 ) ;
#12680 = DIRECTION ( 'NONE',  ( -0.000000000000000000, -0.000000000000000000, -1.000000000000000000 ) ) ;
#12681 = CARTESIAN_POINT ( 'NONE',  ( 28.53771668024168662, -2.080538600569502794, -5.783357778048658027 ) ) ;
#12682 = CARTESIAN_POINT ( 'NONE',  ( 28.88938074516742205, -6.437160617781993999, -4.705209693361168455 ) ) ;
#12683 = DIRECTION ( 'NONE',  ( -0.000000000000000000, -0.000000000000000000, -1.000000000000000000 ) ) ;
#12684 = DIRECTION ( 'NONE',  ( 0.000000000000000000, 0.000000000000000000, -1.000000000000000000 ) ) ;
#12685 = CIRCLE ( 'NONE', #16178, 2.500000000000000000 ) ;
#12686 = CARTESIAN_POINT ( 'NONE',  ( 2.500000000000000000, 2.357898499370432166, -2.385244779468109755E-15 ) ) ;
#12687 = CARTESIAN_POINT ( 'NONE',  ( 2.749999999999992895, -20.49999999999999645, 13.00000000000000178 ) ) ;
#12688 = VECTOR ( 'NONE', #3612, 1000.000000000000000 ) ;
#12689 = CARTESIAN_POINT ( 'NONE',  ( 29.01637427789896151, -7.048830937829683840, -5.783357778048668685 ) ) ;
#12690 = AXIS2_PLACEMENT_3D ( 'NONE', #9473, #17783, #2599 ) ;
#12691 = DIRECTION ( 'NONE',  ( 0.8660254037844432595, 0.4999999999999921174, 0.000000000000000000 ) ) ;
#12692 = FACE_OUTER_BOUND ( 'NONE', #449, .T. ) ;
#12693 = CARTESIAN_POINT ( 'NONE',  ( -23.00000000000000000, -16.21813761408365195, 13.00000000000000178 ) ) ;
#12694 = DIRECTION ( 'NONE',  ( -0.000000000000000000, -0.000000000000000000, -1.000000000000000000 ) ) ;
#12695 = EDGE_CURVE ( 'NONE', #5484, #7696, #7262, .T. ) ;
#12696 = CARTESIAN_POINT ( 'NONE',  ( 32.06776442294927421, -4.173316554281249147, 8.283357778048662468 ) ) ;
#12697 = FACE_BOUND ( 'NONE', #5309, .T. ) ;
#12698 =( BOUNDED_CURVE ( )  B_SPLINE_CURVE ( 2, ( #10185, #12828, #14186, #11447, #1959, #1777, #15457, #6109, #7307 ),
 .UNSPECIFIED., .F., .T. ) 
 B_SPLINE_CURVE_WITH_KNOTS ( ( 3, 2, 2, 2, 3 ),
 ( 0.7884615384615384359, 0.7948717948717948234, 0.8076923076923077094, 0.8205128205128204844, 0.8269230769230769829 ),
 .UNSPECIFIED. ) 
 CURVE ( )  GEOMETRIC_REPRESENTATION_ITEM ( )  RATIONAL_B_SPLINE_CURVE ( ( 0.9330127018922194093, 0.9330127018922194093, 1.000000000000000000, 0.8660254037844387076, 1.000000000000000000, 0.8660254037844387076, 1.000000000000000000, 0.9330127018922187432, 0.9330127018922192983 ) ) 
 REPRESENTATION_ITEM ( '' )  );
#12699 = EDGE_LOOP ( 'NONE', ( #2969, #10491, #11374, #4961, #4255 ) ) ;
#12700 = EDGE_CURVE ( 'NONE', #17201, #13578, #1529, .T. ) ;
#12701 = DIRECTION ( 'NONE',  ( 0.000000000000000000, -0.5027044994213120122, -0.8644583195629319539 ) ) ;
#12702 = DIRECTION ( 'NONE',  ( 0.000000000000000000, 0.000000000000000000, -1.000000000000000000 ) ) ;
#12703 = AXIS2_PLACEMENT_3D ( 'NONE', #316, #9902, #8470 ) ;
#12704 = CARTESIAN_POINT ( 'NONE',  ( -23.00000000000000000, -16.21813761408365195, -13.00000000000000178 ) ) ;
#12705 = ORIENTED_EDGE ( 'NONE', *, *, #13235, .T. ) ;
#12706 = CARTESIAN_POINT ( 'NONE',  ( 27.23882169172318513, -6.009049854935478052, -7.939653947423662927 ) ) ;
#12707 = EDGE_LOOP ( 'NONE', ( #9697, #14622, #11867, #6923 ) ) ;
#12708 = CARTESIAN_POINT ( 'NONE',  ( 28.77978050244509944, -3.315512618508630993, -7.939653947423660263 ) ) ;
#12709 = FACE_OUTER_BOUND ( 'NONE', #4254, .T. ) ;
#12710 = CARTESIAN_POINT ( 'NONE',  ( 3.248936832696172505, -15.16081378324841289, 17.00000000000000000 ) ) ;
#12711 = ORIENTED_EDGE ( 'NONE', *, *, #11811, .T. ) ;
#12712 = CARTESIAN_POINT ( 'NONE',  ( 31.30979230060565044, -7.172264396038955603, -5.783357778048669573 ) ) ;
#12713 = EDGE_CURVE ( 'NONE', #3955, #4061, #4686, .T. ) ;
#12714 = CARTESIAN_POINT ( 'NONE',  ( 18.32374253600956493, -20.38504502893476200, -15.79679025666372283 ) ) ;
#12715 = EDGE_LOOP ( 'NONE', ( #5895, #16367, #12572, #15538 ) ) ;
#12716 = CARTESIAN_POINT ( 'NONE',  ( 31.93198502805756789, -2.935734224299280548, 3.627061608673666893 ) ) ;
#12717 = ADVANCED_FACE ( 'NONE', ( #1706 ), #16290, .F. ) ;
#12718 = AXIS2_PLACEMENT_3D ( 'NONE', #2079, #3513, #13301 ) ;
#12719 = ADVANCED_FACE ( 'NONE', ( #7237 ), #12753, .F. ) ;
#12720 = CARTESIAN_POINT ( 'NONE',  ( 26.41562710823574278, -3.600346414165641828, 3.627061608673666893 ) ) ;
#12721 = CARTESIAN_POINT ( 'NONE',  ( -19.90989778724008019, -21.66613080872904717, 15.52824432210780259 ) ) ;
#12722 = CARTESIAN_POINT ( 'NONE',  ( 29.11750682573587312, -2.010685337989277954, 6.453230759126474148 ) ) ;
#12723 = ORIENTED_EDGE ( 'NONE', *, *, #3322, .T. ) ;
#12724 = EDGE_LOOP ( 'NONE', ( #7163, #7145, #10301 ) ) ;
#12725 = AXIS2_PLACEMENT_3D ( 'NONE', #11275, #13023, #16852 ) ;
#12726 = CARTESIAN_POINT ( 'NONE',  ( 38.15053902264412500, -1.114360604510109765, -9.783357778048662468 ) ) ;
#12727 = ORIENTED_EDGE ( 'NONE', *, *, #7718, .T. ) ;
#12728 = CARTESIAN_POINT ( 'NONE',  ( 27.10304229683147526, -4.771467524953526329, -3.283357778048664688 ) ) ;
#12729 = CARTESIAN_POINT ( 'NONE',  ( 33.55383270609817714, -5.448088258586239796, -3.283357778048667797 ) ) ;
#12730 = CARTESIAN_POINT ( 'NONE',  ( 31.38859741546781379, -7.162769935976271540, -5.783357778048669573 ) ) ;
#12731 = CARTESIAN_POINT ( 'NONE',  ( -4.000000000000000000, 0.1981133338132469168, -1.407451120981426406E-15 ) ) ;
#12732 = APPLICATION_PROTOCOL_DEFINITION ( 'draft international standard', 'automotive_design', 1998, #2977 ) ;
#12733 = CARTESIAN_POINT ( 'NONE',  ( 30.35023428074701002, -1.862166024106576057, -5.783357778048664244 ) ) ;
#12734 = CARTESIAN_POINT ( 'NONE',  ( 29.02054416436834217, -2.659534819136519790, -4.705209693361160461 ) ) ;
#12735 = CARTESIAN_POINT ( 'NONE',  ( 32.29974222271236073, -2.891426744974864071, -3.627061608673662008 ) ) ;
#12736 = EDGE_CURVE ( 'NONE', #6730, #11134, #12114, .T. ) ;
#12737 = DIRECTION ( 'NONE',  ( -0.9928203230275512992, -0.1196152422706610319, -9.614813431917826478E-17 ) ) ;
#12738 = DIRECTION ( 'NONE',  ( -1.000000000000000000, -0.000000000000000000, -0.000000000000000000 ) ) ;
#12739 = CARTESIAN_POINT ( 'NONE',  ( 30.30787278169304244, -6.266260340387784566, 6.861505862736157368 ) ) ;
#12740 = CLOSED_SHELL ( 'NONE', ( #17156, #8212, #7574, #15108, #5369, #2417, #3945, #16991, #4766, #17044, #1905, #8185, #2697, #3744, #465, #15842, #7735, #3209, #13358, #3027, #389, #9794, #8013, #5549, #2401, #5911, #13949, #7374, #16082, #14983, #3844, #9371, #13133, #17062, #7320, #16317, #7535, #17168, #11977, #444, #10694, #14013, #365, #7373, #1969, #14431, #12797, #13182, #8005, #5090, #8278, #10760, #15653, #17796, #13034, #15466, #16704 ) ) ;
#12741 = ORIENTED_EDGE ( 'NONE', *, *, #17889, .F. ) ;
#12742 = EDGE_LOOP ( 'NONE', ( #8595, #14439, #9733, #1792, #11155, #5794, #16191, #3965, #4659, #15495, #2314, #1617, #3058, #1565, #14583, #1354, #4479, #9442, #8807, #3599, #13493, #204, #9032, #14746, #16028, #4174, #17305, #8040 ) ) ;
#12743 = CARTESIAN_POINT ( 'NONE',  ( 29.01637427789896151, -7.048830937829683840, 5.783357778048658027 ) ) ;
#12744 = FILL_AREA_STYLE_COLOUR ( '', #919 ) ;
#12745 = CARTESIAN_POINT ( 'NONE',  ( 45.50000000000000000, -16.03270077640482683, 2.787981825772262390 ) ) ;
#12746 = VECTOR ( 'NONE', #10178, 1000.000000000000000 ) ;
#12747 = ORIENTED_EDGE ( 'NONE', *, *, #3011, .T. ) ;
#12748 = FILL_AREA_STYLE_COLOUR ( '', #3581 ) ;
#12749 = ORIENTED_EDGE ( 'NONE', *, *, #2508, .T. ) ;
#12750 = CARTESIAN_POINT ( 'NONE',  ( -3.248936832696171617, 7.999999999999989342, 17.00000000000000000 ) ) ;
#12751 = FACE_OUTER_BOUND ( 'NONE', #12635, .T. ) ;
#12752 = EDGE_CURVE ( 'NONE', #17749, #2915, #8411, .T. ) ;
#12753 = CYLINDRICAL_SURFACE ( 'NONE', #1810, 2.499999999999999112 ) ;
#12754 = CARTESIAN_POINT ( 'NONE',  ( 26.32044349065828115, -7.243571858916999950, -6.694428052743685242 ) ) ;
#12755 = CARTESIAN_POINT ( 'NONE',  ( 32.38298487551052318, -4.135338714860305132, -8.283357778048662468 ) ) ;
#12756 = VERTEX_POINT ( 'NONE', #5583 ) ;
#12757 = CARTESIAN_POINT ( 'NONE',  ( 26.94172295629870462, -6.971623697019761146, -7.033357778048666908 ) ) ;
#12758 = CARTESIAN_POINT ( 'NONE',  ( 15.92260893619738837, -28.39189527176317540, -6.000000000000000000 ) ) ;
#12759 = CARTESIAN_POINT ( 'NONE',  ( 3.538288549924106796, -15.34800872113743431, 16.99955934415557479 ) ) ;
#12760 =( NAMED_UNIT ( * ) SI_UNIT ( $, .STERADIAN. ) SOLID_ANGLE_UNIT ( ) );
#12761 = CARTESIAN_POINT ( 'NONE',  ( 30.27725608814395031, -6.896919580145944195, -5.783357778048668685 ) ) ;
#12762 = EDGE_LOOP ( 'NONE', ( #3637, #10717, #4049, #14207 ) ) ;
#12763 = CARTESIAN_POINT ( 'NONE',  ( 25.88432464927661769, -3.805096980563277498, -7.814840548041910750 ) ) ;
#12764 = AXIS2_PLACEMENT_3D ( 'NONE', #9244, #14790, #6449 ) ;
#12765 = DIRECTION ( 'NONE',  ( -0.000000000000000000, -0.000000000000000000, 1.000000000000000000 ) ) ;
#12766 = VERTEX_POINT ( 'NONE', #9839 ) ;
#12767 = EDGE_LOOP ( 'NONE', ( #16503, #1970, #491, #10863, #8445 ) ) ;
#12768 = AXIS2_PLACEMENT_3D ( 'NONE', #4195, #15337, #8539 ) ;
#12769 = ORIENTED_EDGE ( 'NONE', *, *, #654, .F. ) ;
#12770 = CARTESIAN_POINT ( 'NONE',  ( 28.24571643650507369, -4.633797857156355171, 3.627061608673664228 ) ) ;
#12771 = PLANE ( 'NONE',  #14297 ) ;
#12772 = CARTESIAN_POINT ( 'NONE',  ( 46.86575133767495061, -2.390451368237048069, -5.783357778048661579 ) ) ;
#12773 = CARTESIAN_POINT ( 'NONE',  ( -9.647391702364178201, 16.07861560120820243, -16.78732711007196698 ) ) ;
#12774 = EDGE_CURVE ( 'NONE', #43, #5433, #12791, .T. ) ;
#12775 = DIRECTION ( 'NONE',  ( 0.000000000000000000, 0.000000000000000000, 1.000000000000000000 ) ) ;
#12777 = AXIS2_PLACEMENT_3D ( 'NONE', #1999, #13227, #12956 ) ;
#12776 = CARTESIAN_POINT ( 'NONE',  ( 32.80318959510331212, -2.203800746085299522, -4.705209693361160461 ) ) ;
#12778 = CARTESIAN_POINT ( 'NONE',  ( 31.83134908525019213, -4.201799933639492224, -8.283357778048662468 ) ) ;
#12779 = CARTESIAN_POINT ( 'NONE',  ( -1.917618200156724081E-28, -7.000000000000001776, 17.00000000000000000 ) ) ;
#12780 = DIRECTION ( 'NONE',  ( 0.000000000000000000, 0.000000000000000000, -1.000000000000000000 ) ) ;
#12781 = CARTESIAN_POINT ( 'NONE',  ( -8.876997858717690093, 16.38553564496311310, 16.83638096351226920 ) ) ;
#12782 = CIRCLE ( 'NONE', #16271, 10.50000000000000000 ) ;
#12783 = ORIENTED_EDGE ( 'NONE', *, *, #4556, .F. ) ;
#12784 = CARTESIAN_POINT ( 'NONE',  ( 31.71314141467879111, -4.216041623526076698, -3.627061608673664672 ) ) ;
#12785 = DIRECTION ( 'NONE',  ( 1.224646799147353207E-16, -1.000000000000000000, 0.000000000000000000 ) ) ;
#12786 = FACE_OUTER_BOUND ( 'NONE', #9896, .T. ) ;
#12787 = CARTESIAN_POINT ( 'NONE',  ( 27.17934203385504333, -30.00000000000000355, 0.000000000000000000 ) ) ;
#12788 = LINE ( 'NONE', #4360, #12975 ) ;
#12789 = CARTESIAN_POINT ( 'NONE',  ( 29.54600080245929306, -4.477139269648729325, 8.283357778048662468 ) ) ;
#12790 = CARTESIAN_POINT ( 'NONE',  ( 26.34117031759772942, -2.982346454214467535, -4.705209693361161349 ) ) ;
#12791 = CIRCLE ( 'NONE', #15106, 10.50000000000000000 ) ;
#12792 = ORIENTED_EDGE ( 'NONE', *, *, #3548, .T. ) ;
#12793 = EDGE_LOOP ( 'NONE', ( #12711, #1591, #3881, #7205 ) ) ;
#12794 = CARTESIAN_POINT ( 'NONE',  ( 5.781152949374531502, 1.605699403978890993, -3.000000000000000888 ) ) ;
#12795 = CARTESIAN_POINT ( 'NONE',  ( -2.016448651773435938E-27, -20.49999999999999645, 6.000000000000000000 ) ) ;
#12796 = CIRCLE ( 'NONE', #8449, 2.749999999999992895 ) ;
#12797 = ADVANCED_FACE ( 'NONE', ( #11100 ), #16668, .T. ) ;
#12798 = ORIENTED_EDGE ( 'NONE', *, *, #11729, .F. ) ;
#12799 = CARTESIAN_POINT ( 'NONE',  ( -17.07594129529364579, -14.18356557013591868, -15.98851070825981324 ) ) ;
#12800 = ADVANCED_FACE ( 'NONE', ( #3583 ), #6705, .T. ) ;
#12801 = ORIENTED_EDGE ( 'NONE', *, *, #5177, .F. ) ;
#12802 = CARTESIAN_POINT ( 'NONE',  ( 26.37178701114681800, -2.351687214456304797, -5.783357778048658915 ) ) ;
#12803 = CARTESIAN_POINT ( 'NONE',  ( 30.88577694472199298, -6.196634301449400084, -6.861505862736166250 ) ) ;
#12804 = FACE_OUTER_BOUND ( 'NONE', #11370, .T. ) ;
#12805 = LINE ( 'NONE', #400, #3178 ) ;
#12806 = VECTOR ( 'NONE', #497, 1000.000000000000000 ) ;
#12807 = DIRECTION ( 'NONE',  ( 0.000000000000000000, 0.000000000000000000, -1.000000000000000000 ) ) ;
#12808 = VECTOR ( 'NONE', #236, 1000.000000000000000 ) ;
#12809 = CARTESIAN_POINT ( 'NONE',  ( 30.44283453230164227, -2.188368138933637574, -4.533357778048659803 ) ) ;
#12810 = VECTOR ( 'NONE', #12397, 1000.000000000000227 ) ;
#12811 =( BOUNDED_SURFACE ( )  B_SPLINE_SURFACE ( 1, 2, ( 
 ( #16588, #4170, #6234, #15675, #4778, #3252, #10489, #14322, #1904, #13219, #10300, #4600, #17143, #530, #8956, #16050, #15767, #6146, #17424, #10218, #7513, #15854, #7606, #11846, #8789, #8872, #6045, #2176, #7428, #3427, #13036, #14500, #796, #12944, #4865, #10395, #6323, #4957, #3619, #17238, #9141, #17046, #14680, #15947, #11574, #2085, #3517, #2261, #13132, #4692, #9051, #712, #14406, #14601, #3341, #1988, #623, #7693, #12864, #451, #11755, #17326, #5952, #11478, #10122, #11672, #9803, #11151, #2602, #888, #16134, #14768, #14934, #17786, #15354, #3961, #10827, #2512, #16721, #9392, #1066, #5307, #13492, #2353, #5048, #16221, #3788, #10738, #5218, #6678, #8129, #3696, #16313, #7872, #10570, #12025, #13403, #6587, #4292, #12209, #1155, #12544, #9476, #984, #15015, #13308, #16395, #9220, #6513, #5130, #13574, #7779, #17611, #10651, #9310, #14849, #2437, #7958, #12113, #17695, #3879, #8038, #13899, #1491, #7024, #126, #5637, #6421, #11939, #17529, #15626, #577, #7295, #10261, #14001, #5724, #9897, #10077, #12814, #5818, #3301, #488, #11341, #3202, #15448, #1584, #3113, #6095, #12991, #11625, #406, #8468, #4554 ),
 ( #11241, #14274, #17190, #309, #17094, #16818, #5912, #4736, #5998, #1861, #3030, #215, #7206, #8553, #1765, #2933, #7390, #12905, #7468, #4648, #14085, #10174, #7117, #11526, #4383, #1671, #16917, #8744, #12631, #12716, #4472, #9987, #15532, #8644, #14173, #11436, #17002, #15726, #8830, #14363, #1948, #11712, #13087, #666, #2035, #3383, #17283, #6189, #4818, #7560, #15809, #8917, #14453, #3956, #4140, #6850, #17865, #15276, #12467, #5387, #15194, #9470, #13570, #15103, #142, #7045, #12561, #12376, #2507, #16556, #6766, #2776, #1151, #10904, #16738, #6672, #9556, #17943, #10823, #16391, #9644, #12204, #5655, #8297, #15010, #11167, #17781, #13916, #56, #2597, #13825, #5567, #1511, #1413, #8123, #11085, #5476, #16471, #16650, #13657, #1246, #2688, #6936, #4225, #8386, #9725, #2858, #8033, #4310, #10997, #12299, #14931, #5302, #4042, #8217, #13748, #1326, #16217, #3781, #15102, #6671, #6506, #1061, #2432, #10820, #12375, #17689, #8032, #1325, #12108, #9386, #12202, #9469, #13745, #17605, #10732, #7952, #4039, #16390, #17942, #5213, #13569, #6848, #16306, #14929, #17780, #15009, #5474, #5125, #3874, #13486, #9555, #10646 ) ),
 .UNSPECIFIED., .F., .F., .T. ) 
 B_SPLINE_SURFACE_WITH_KNOTS ( ( 2, 2 ),
 ( 3, 2, 2, 2, 2, 2, 2, 2, 2, 2, 2, 2, 2, 2, 2, 2, 2, 2, 2, 2, 2, 2, 2, 2, 2, 2, 2, 2, 2, 2, 2, 2, 2, 2, 2, 2, 2, 2, 2, 2, 2, 2, 2, 2, 2, 2, 2, 2, 2, 2, 2, 2, 2, 2, 2, 2, 2, 2, 2, 2, 2, 2, 2, 2, 2, 2, 2, 2, 2, 2, 2, 2, 2, 2, 2, 2, 3 ),
 ( 0.000000000000000000, 1.000000000000000000 ),
 ( 0.000000000000000000, 0.01282051282051282007, 0.02564102564102564014, 0.03846153846153846367, 0.05128205128205128027, 0.06410256410256409687, 0.07692307692307692735, 0.08974358974358974395, 0.1025641025641025605, 0.1153846153846153910, 0.1282051282051281937, 0.1410256410256410242, 0.1538461538461538547, 0.1666666666666666574, 0.1794871794871794879, 0.1923076923076923184, 0.2051282051282051211, 0.2179487179487179516, 0.2307692307692307820, 0.2435897435897435848, 0.2564102564102563875, 0.2692307692307692180, 0.2820512820512820484, 0.2948717948717948789, 0.3076923076923077094, 0.3205128205128205399, 0.3333333333333333148, 0.3461538461538461453, 0.3589743589743589758, 0.3717948717948718063, 0.3846153846153846367, 0.3974358974358974117, 0.4102564102564102422, 0.4230769230769230727, 0.4358974358974359031, 0.4487179487179487336, 0.4615384615384615641, 0.4743589743589743390, 0.4871794871794871695, 0.5000000000000000000, 0.5128205128205127750, 0.5256410256410256610, 0.5384615384615384359, 0.5512820512820513219, 0.5641025641025640969, 0.5769230769230768718, 0.5897435897435897578, 0.6025641025641025328, 0.6153846153846154188, 0.6282051282051281937, 0.6410256410256410797, 0.6538461538461538547, 0.6666666666666666297, 0.6794871794871795156, 0.6923076923076922906, 0.7051282051282051766, 0.7179487179487179516, 0.7307692307692307265, 0.7435897435897436125, 0.7564102564102563875, 0.7692307692307692735, 0.7820512820512820484, 0.7948717948717948234, 0.8076923076923077094, 0.8205128205128204844, 0.8333333333333333703, 0.8461538461538461453, 0.8589743589743589203, 0.8717948717948718063, 0.8846153846153845812, 0.8974358974358974672, 0.9102564102564102422, 0.9230769230769231282, 0.9358974358974359031, 0.9487179487179486781, 0.9615384615384615641, 0.9690837704703162414 ),
 .UNSPECIFIED. ) 
 GEOMETRIC_REPRESENTATION_ITEM ( )  RATIONAL_B_SPLINE_SURFACE ( (
 ( 1.000000000000000000, 0.8660254037844387076, 1.000000000000000000, 0.8660254037844387076, 1.000000000000000000, 0.8660254037844387076, 1.000000000000000000, 0.8660254037844387076, 1.000000000000000000, 0.8660254037844387076, 1.000000000000000000, 0.8660254037844387076, 1.000000000000000000, 0.8660254037844387076, 1.000000000000000000, 0.8660254037844387076, 1.000000000000000000, 0.8660254037844387076, 1.000000000000000000, 0.8660254037844387076, 1.000000000000000000, 0.8660254037844387076, 1.000000000000000000, 0.8660254037844387076, 1.000000000000000000, 0.8660254037844387076, 1.000000000000000000, 0.8660254037844387076, 1.000000000000000000, 0.8660254037844387076, 1.000000000000000000, 0.8660254037844387076, 1.000000000000000000, 0.8660254037844387076, 1.000000000000000000, 0.8660254037844387076, 1.000000000000000000, 0.8660254037844387076, 1.000000000000000000, 0.8660254037844387076, 1.000000000000000000, 0.8660254037844387076, 1.000000000000000000, 0.8660254037844387076, 1.000000000000000000, 0.8660254037844387076, 1.000000000000000000, 0.8660254037844387076, 1.000000000000000000, 0.8660254037844387076, 1.000000000000000000, 0.8660254037844387076, 1.000000000000000000, 0.8660254037844387076, 1.000000000000000000, 0.8660254037844387076, 1.000000000000000000, 0.8660254037844387076, 1.000000000000000000, 0.8660254037844387076, 1.000000000000000000, 0.8660254037844387076, 1.000000000000000000, 0.8660254037844387076, 1.000000000000000000, 0.8660254037844387076, 1.000000000000000000, 0.8660254037844387076, 1.000000000000000000, 0.8660254037844387076, 1.000000000000000000, 0.8660254037844387076, 1.000000000000000000, 0.8660254037844387076, 1.000000000000000000, 0.8660254037844387076, 1.000000000000000000, 0.8660254037844387076, 1.000000000000000000, 0.8660254037844387076, 1.000000000000000000, 0.8660254037844387076, 1.000000000000000000, 0.8660254037844387076, 1.000000000000000000, 0.8660254037844387076, 1.000000000000000000, 0.8660254037844387076, 1.000000000000000000, 0.8660254037844387076, 1.000000000000000000, 0.8660254037844387076, 1.000000000000000000, 0.8660254037844387076, 1.000000000000000000, 0.8660254037844387076, 1.000000000000000000, 0.8660254037844387076, 1.000000000000000000, 0.8660254037844387076, 1.000000000000000000, 0.8660254037844387076, 1.000000000000000000, 0.8660254037844387076, 1.000000000000000000, 0.8660254037844387076, 1.000000000000000000, 0.8660254037844387076, 1.000000000000000000, 0.8660254037844387076, 1.000000000000000000, 0.8660254037844387076, 1.000000000000000000, 0.8660254037844387076, 1.000000000000000000, 0.8660254037844387076, 1.000000000000000000, 0.8660254037844387076, 1.000000000000000000, 0.8660254037844387076, 1.000000000000000000, 0.8660254037844387076, 1.000000000000000000, 0.8660254037844387076, 1.000000000000000000, 0.8660254037844387076, 1.000000000000000000, 0.8660254037844387076, 1.000000000000000000, 0.8660254037844387076, 1.000000000000000000, 0.8660254037844387076, 1.000000000000000000, 0.8660254037844387076, 1.000000000000000000, 0.8660254037844387076, 1.000000000000000000, 0.8660254037844387076, 1.000000000000000000, 0.8660254037844387076, 1.000000000000000000, 0.8660254037844387076, 1.000000000000000000, 0.8660254037844387076, 1.000000000000000000, 0.8660254037844387076, 1.000000000000000000, 0.8660254037844387076, 1.000000000000000000, 0.8660254037844387076, 1.000000000000000000, 0.9211513820375816231, 0.9351129643698559146),
 ( 1.000000000000000000, 0.8660254037844387076, 1.000000000000000000, 0.8660254037844387076, 1.000000000000000000, 0.8660254037844387076, 1.000000000000000000, 0.8660254037844387076, 1.000000000000000000, 0.8660254037844387076, 1.000000000000000000, 0.8660254037844387076, 1.000000000000000000, 0.8660254037844387076, 1.000000000000000000, 0.8660254037844387076, 1.000000000000000000, 0.8660254037844387076, 1.000000000000000000, 0.8660254037844387076, 1.000000000000000000, 0.8660254037844387076, 1.000000000000000000, 0.8660254037844387076, 1.000000000000000000, 0.8660254037844387076, 1.000000000000000000, 0.8660254037844387076, 1.000000000000000000, 0.8660254037844387076, 1.000000000000000000, 0.8660254037844387076, 1.000000000000000000, 0.8660254037844387076, 1.000000000000000000, 0.8660254037844387076, 1.000000000000000000, 0.8660254037844387076, 1.000000000000000000, 0.8660254037844387076, 1.000000000000000000, 0.8660254037844387076, 1.000000000000000000, 0.8660254037844387076, 1.000000000000000000, 0.8660254037844387076, 1.000000000000000000, 0.8660254037844387076, 1.000000000000000000, 0.8660254037844387076, 1.000000000000000000, 0.8660254037844387076, 1.000000000000000000, 0.8660254037844387076, 1.000000000000000000, 0.8660254037844387076, 1.000000000000000000, 0.8660254037844387076, 1.000000000000000000, 0.8660254037844387076, 1.000000000000000000, 0.8660254037844387076, 1.000000000000000000, 0.8660254037844387076, 1.000000000000000000, 0.8660254037844387076, 1.000000000000000000, 0.8660254037844387076, 1.000000000000000000, 0.8660254037844387076, 1.000000000000000000, 0.8660254037844387076, 1.000000000000000000, 0.8660254037844387076, 1.000000000000000000, 0.8660254037844387076, 1.000000000000000000, 0.8660254037844387076, 1.000000000000000000, 0.8660254037844387076, 1.000000000000000000, 0.8660254037844387076, 1.000000000000000000, 0.8660254037844387076, 1.000000000000000000, 0.8660254037844387076, 1.000000000000000000, 0.8660254037844387076, 1.000000000000000000, 0.8660254037844387076, 1.000000000000000000, 0.8660254037844387076, 1.000000000000000000, 0.8660254037844387076, 1.000000000000000000, 0.8660254037844387076, 1.000000000000000000, 0.8660254037844387076, 1.000000000000000000, 0.8660254037844387076, 1.000000000000000000, 0.8660254037844387076, 1.000000000000000000, 0.8660254037844387076, 1.000000000000000000, 0.8660254037844387076, 1.000000000000000000, 0.8660254037844387076, 1.000000000000000000, 0.8660254037844387076, 1.000000000000000000, 0.8660254037844387076, 1.000000000000000000, 0.8660254037844387076, 1.000000000000000000, 0.8660254037844387076, 1.000000000000000000, 0.8660254037844387076, 1.000000000000000000, 0.8660254037844387076, 1.000000000000000000, 0.8660254037844387076, 1.000000000000000000, 0.8660254037844387076, 1.000000000000000000, 0.8660254037844387076, 1.000000000000000000, 0.8660254037844387076, 1.000000000000000000, 0.8660254037844387076, 1.000000000000000000, 0.8660254037844387076, 1.000000000000000000, 0.8660254037844387076, 1.000000000000000000, 0.8660254037844387076, 1.000000000000000000, 0.8660254037844387076, 1.000000000000000000, 0.8660254037844387076, 1.000000000000000000, 0.8660254037844387076, 1.000000000000000000, 0.8660254037844387076, 1.000000000000000000, 0.8660254037844387076, 1.000000000000000000, 0.8660254037844387076, 1.000000000000000000, 0.8660254037844387076, 1.000000000000000000, 0.9211513820375816231, 0.9351129643698559146) ) ) 
 REPRESENTATION_ITEM ( '' )  SURFACE ( )  );
#12812 = CARTESIAN_POINT ( 'NONE',  ( -2.500000000000000888, 0.000000000000000000, -4.674599999999997202 ) ) ;
#12813 = ORIENTED_EDGE ( 'NONE', *, *, #17646, .T. ) ;
#12814 = CARTESIAN_POINT ( 'NONE',  ( 26.15738093914773543, -4.885401043216321959, 3.283357778048664244 ) ) ;
#12815 = VECTOR ( 'NONE', #3306, 1000.000000000000000 ) ;
#12816 = DIRECTION ( 'NONE',  ( -0.000000000000000000, -0.000000000000000000, 1.000000000000000000 ) ) ;
#12817 = CARTESIAN_POINT ( 'NONE',  ( -20.83887142315839469, -22.08617648736154493, 15.35754594250728999 ) ) ;
#12818 = CARTESIAN_POINT ( 'NONE',  ( -10.27627944162886209, -4.200961894323246071, -2.000000000000000000 ) ) ;
#12819 = VERTEX_POINT ( 'NONE', #11720 ) ;
#12820 = CARTESIAN_POINT ( 'NONE',  ( 0.000000000000000000, 0.000000000000000000, -2.000000000000000000 ) ) ;
#12821 = TOROIDAL_SURFACE ( 'NONE', #7344, 5.384454397937117776, 0.5155456020628805813 ) ;
#12822 = ORIENTED_EDGE ( 'NONE', *, *, #8861, .T. ) ;
#12823 = FACE_OUTER_BOUND ( 'NONE', #6790, .T. ) ;
#12824 = ADVANCED_FACE ( 'NONE', ( #763, #17486 ), #16101, .T. ) ;
#12825 = CARTESIAN_POINT ( 'NONE',  ( -34.91600907648203389, -11.88801210197604341, -11.56671555609732671 ) ) ;
#12826 = EDGE_LOOP ( 'NONE', ( #12119, #2910, #13575, #9986 ) ) ;
#12827 = EDGE_LOOP ( 'NONE', ( #9313, #5341, #17918, #14261 ) ) ;
#12828 = CARTESIAN_POINT ( 'NONE',  ( 26.61823960964035507, -2.311797680896151341, -6.453230759126464378 ) ) ;
#12829 = CARTESIAN_POINT ( 'NONE',  ( 26.39823381822651882, -6.110324093391315436, -3.627061608673668225 ) ) ;
#12830 = CARTESIAN_POINT ( 'NONE',  ( 30.52163964716380917, -2.178873678870954400, -4.533357778048659803 ) ) ;
#12831 = VECTOR ( 'NONE', #11494, 1000.000000000000000 ) ;
#12832 = CARTESIAN_POINT ( 'NONE',  ( -4.000000000000000000, 2.309401076758501592, -0.4999999999999963363 ) ) ;
#12833 = PRODUCT_CONTEXT ( 'NONE', #13956, 'mechanical' ) ;
#12834 = CARTESIAN_POINT ( 'NONE',  ( 33.47428445112562656, -1.485779673698265135, 5.113484796970859669 ) ) ;
#12835 = EDGE_CURVE ( 'NONE', #12145, #8066, #3247, .T. ) ;
#12836 = CARTESIAN_POINT ( 'NONE',  ( 27.63266882139180680, -2.199775856772564708, -5.783357778048658027 ) ) ;
#12837 = CARTESIAN_POINT ( 'NONE',  ( -4.203833317240879275, -1.627343821129590307, -3.297273115243891439 ) ) ;
#12838 = DIRECTION ( 'NONE',  ( -1.000000000000000000, 2.131628207280300558E-14, 0.000000000000000000 ) ) ;
#12839 = CARTESIAN_POINT ( 'NONE',  ( 29.18947247604338102, -3.066280307211263434, 3.283357778048666464 ) ) ;
#12840 = CARTESIAN_POINT ( 'NONE',  ( 29.76058531221316628, -5.705227139567997874, 3.627061608673662896 ) ) ;
#12841 = ORIENTED_EDGE ( 'NONE', *, *, #14940, .T. ) ;
#12842 = CARTESIAN_POINT ( 'NONE',  ( 25.95642634701329499, -4.403549397486667516, 7.880302681851837576 ) ) ;
#12843 = ORIENTED_EDGE ( 'NONE', *, *, #9625, .F. ) ;
#12844 = CARTESIAN_POINT ( 'NONE',  ( 27.93049598394382116, -4.671775696577297410, 7.939653947423662039 ) ) ;
#12845 = CARTESIAN_POINT ( 'NONE',  ( 32.37175601071535169, -5.590505156207296267, -3.283357778048667797 ) ) ;
#12846 = DIRECTION ( 'NONE',  ( -0.000000000000000000, -0.000000000000000000, -1.000000000000000000 ) ) ;
#12847 = VERTEX_POINT ( 'NONE', #9187 ) ;
#12848 = CARTESIAN_POINT ( 'NONE',  ( 28.64916707261694384, -6.765910400363817523, -4.533357778048668685 ) ) ;
#12849 = VERTEX_POINT ( 'NONE', #16947 ) ;
#12850 = PLANE ( 'NONE',  #11263 ) ;
#12851 = EDGE_CURVE ( 'NONE', #11613, #1319, #8683, .T. ) ;
#12852 = CIRCLE ( 'NONE', #1556, 12.50000000000000000 ) ;
#12853 = DIRECTION ( 'NONE',  ( -1.000000000000000000, -0.000000000000000000, -0.000000000000000000 ) ) ;
#12854 = AXIS2_PLACEMENT_3D ( 'NONE', #2248, #9037, #3506 ) ;
#12855 = CARTESIAN_POINT ( 'NONE',  ( 4.000000000000000000, 2.309401076758498483, -3.133295621305380863 ) ) ;
#12856 = CARTESIAN_POINT ( 'NONE',  ( 33.19286683830256379, -2.783822866615540903, -7.939653947423660263 ) ) ;
#12857 = LINE ( 'NONE', #7339, #8957 ) ;
#12858 = DIRECTION ( 'NONE',  ( 0.000000000000000000, 0.000000000000000000, 1.000000000000000000 ) ) ;
#12859 = EDGE_CURVE ( 'NONE', #14228, #6328, #9273, .T. ) ;
#12860 =( LENGTH_UNIT ( ) NAMED_UNIT ( * ) SI_UNIT ( .MILLI., .METRE. ) );
#12861 = CARTESIAN_POINT ( 'NONE',  ( 31.93198502805756789, -2.935734224299280548, -7.939653947423660263 ) ) ;
#12862 = EDGE_LOOP ( 'NONE', ( #9829, #6268 ) ) ;
#12863 = CARTESIAN_POINT ( 'NONE',  ( 34.91600907648203389, -11.88801210197604341, -12.00000000000000000 ) ) ;
#12864 = CARTESIAN_POINT ( 'NONE',  ( 30.61929490284659394, -6.528548903775525325, 7.033357778048657138 ) ) ;
#12865 = ADVANCED_FACE ( 'NONE', ( #2142, #17388 ), #14733, .F. ) ;
#12866 = ORIENTED_EDGE ( 'NONE', *, *, #14708, .T. ) ;
#12867 = EDGE_LOOP ( 'NONE', ( #6756, #7443, #14643, #3020 ) ) ;
#12868 = EDGE_LOOP ( 'NONE', ( #15243, #8139, #13153, #4337 ) ) ;
#12869 = CARTESIAN_POINT ( 'NONE',  ( 30.23341599105502908, -5.648260380436596506, 3.627061608673662896 ) ) ;
#12870 = CARTESIAN_POINT ( 'NONE',  ( 26.34117031759772942, -2.982346454214467535, -4.705209693361161349 ) ) ;
#12871 = CARTESIAN_POINT ( 'NONE',  ( 20.00000000000000355, -30.00000000000000355, -17.00000000000000000 ) ) ;
#12872 = DIRECTION ( 'NONE',  ( 0.000000000000000000, 0.000000000000000000, -1.000000000000000000 ) ) ;
#12873 = ADVANCED_FACE ( 'NONE', ( #15909 ), #4826, .T. ) ;
#12874 = CARTESIAN_POINT ( 'NONE',  ( 1.296864337298335788E-21, -1.182044466681725685E-21, -6.899999999999998579 ) ) ;
#12875 = CARTESIAN_POINT ( 'NONE',  ( 32.08959525433819238, -2.916745304588811649, -7.939653947423660263 ) ) ;
#12876 = CARTESIAN_POINT ( 'NONE',  ( 29.16815758536418102, -2.004582921727632971, 5.783357778048662468 ) ) ;
#12877 = LINE ( 'NONE', #12961, #4980 ) ;
#12878 = CARTESIAN_POINT ( 'NONE',  ( 27.81599742762458050, -2.504850134108091098, -7.033357778048658027 ) ) ;
#12879 = EDGE_LOOP ( 'NONE', ( #11199, #10222, #16769, #14639, #2492, #6099 ) ) ;
#12880 = CARTESIAN_POINT ( 'NONE',  ( 33.54323074294813267, -5.249493066516778050, -7.939653947423664704 ) ) ;
#12881 = DIRECTION ( 'NONE',  ( 0.000000000000000000, 0.000000000000000000, 1.000000000000000000 ) ) ;
#12882 = CARTESIAN_POINT ( 'NONE',  ( 26.87859896403794835, -7.316587507915443211, -6.453230759126474148 ) ) ;
#12883 = DIRECTION ( 'NONE',  ( -1.000000000000000000, 0.000000000000000000, 0.000000000000000000 ) ) ;
#12884 = PLANE ( 'NONE',  #823 ) ;
#12885 = EDGE_CURVE ( 'NONE', #11393, #4229, #9322, .T. ) ;
#12886 = CARTESIAN_POINT ( 'NONE',  ( 28.05993251931039012, -3.202367565343739564, 8.283357778048664244 ) ) ;
#12887 = DIRECTION ( 'NONE',  ( -0.1196152422706610735, 0.9928203230275511881, 0.000000000000000000 ) ) ;
#12888 = ORIENTED_EDGE ( 'NONE', *, *, #12316, .F. ) ;
#12889 = DIRECTION ( 'NONE',  ( 1.000000000000000000, 0.000000000000000000, -0.000000000000000000 ) ) ;
#12890 = ORIENTED_EDGE ( 'NONE', *, *, #16124, .T. ) ;
#12891 = VERTEX_POINT ( 'NONE', #13365 ) ;
#12892 = CARTESIAN_POINT ( 'NONE',  ( 29.32081432955537537, -3.050456207659999475, -3.283357778048662023 ) ) ;
#12893 = ADVANCED_FACE ( 'NONE', ( #7741 ), #7926, .F. ) ;
#12894 = EDGE_LOOP ( 'NONE', ( #1720, #16824, #14667, #4291, #10794, #6781, #11113, #6219, #5244, #16699, #17328, #12888, #2871, #13136, #5091, #9393, #10104, #3284, #890, #7827, #5447, #6124, #641, #7760, #609, #16545, #414, #38 ) ) ;
#12895 = CYLINDRICAL_SURFACE ( 'NONE', #1802, 6.000000000000000888 ) ;
#12896 = CARTESIAN_POINT ( 'NONE',  ( 26.70901672940806648, -4.818939824437135755, -8.283357778048662468 ) ) ;
#12897 =( BOUNDED_CURVE ( )  B_SPLINE_CURVE ( 2, ( #11435, #8829, #3200, #8642, #15725, #1762, #14452, #8742, #1860 ),
 .UNSPECIFIED., .F., .T. ) 
 B_SPLINE_CURVE_WITH_KNOTS ( ( 3, 2, 2, 2, 3 ),
 ( 0.5576923076923077094, 0.5641025641025640969, 0.5769230769230768718, 0.5897435897435897578, 0.5961538461538461453 ),
 .UNSPECIFIED. ) 
 CURVE ( )  GEOMETRIC_REPRESENTATION_ITEM ( )  RATIONAL_B_SPLINE_CURVE ( ( 0.9330127018922194093, 0.9330127018922194093, 1.000000000000000000, 0.8660254037844387076, 1.000000000000000000, 0.8660254037844387076, 1.000000000000000000, 0.9330127018922194093, 0.9330127018922194093 ) ) 
 REPRESENTATION_ITEM ( '' )  );
#12898 = CARTESIAN_POINT ( 'NONE',  ( 29.51982165028991645, -6.361204938940122844, -4.705209693361168455 ) ) ;
#12899 = CARTESIAN_POINT ( 'NONE',  ( -1.317756351988338626, 3.857995168970202116, -0.04852650426601485406 ) ) ;
#12900 = LINE ( 'NONE', #4731, #11853 ) ;
#12901 = DIRECTION ( 'NONE',  ( -0.8660254037844363761, 0.5000000000000038858, 0.000000000000000000 ) ) ;
#12902 = CARTESIAN_POINT ( 'NONE',  ( 30.61177514885987350, -5.802548093181622235, -8.283357778048662468 ) ) ;
#12903 = DIRECTION ( 'NONE',  ( -0.000000000000000000, -0.000000000000000000, -1.000000000000000000 ) ) ;
#12904 = EDGE_CURVE ( 'NONE', #397, #2657, #1110, .T. ) ;
#12905 = CARTESIAN_POINT ( 'NONE',  ( 32.56242593318007295, -2.859778545457410281, 3.627061608673666893 ) ) ;
#12906 = DIRECTION ( 'NONE',  ( -0.000000000000000000, -0.000000000000000000, -1.000000000000000000 ) ) ;
#12907 = CARTESIAN_POINT ( 'NONE',  ( 32.95080301609915097, -1.548848848676412260, 5.783357778048663356 ) ) ;
#12908 = ORIENTED_EDGE ( 'NONE', *, *, #13451, .F. ) ;
#12909 = CARTESIAN_POINT ( 'NONE',  ( -6.935828204433864386, -17.68137362934027479, 16.94363565911716663 ) ) ;
#12910 = ORIENTED_EDGE ( 'NONE', *, *, #2636, .F. ) ;
#12911 = CARTESIAN_POINT ( 'NONE',  ( 8.809730593168891843, -18.96833375928839516, -16.83727734034771473 ) ) ;
#12912 = LINE ( 'NONE', #495, #7580 ) ;
#12913 = ORIENTED_EDGE ( 'NONE', *, *, #12982, .F. ) ;
#12914 = CARTESIAN_POINT ( 'NONE',  ( 23.02601376483258022, 3.965314980223224151, 0.000000000000000000 ) ) ;
#12915 = CARTESIAN_POINT ( 'NONE',  ( 33.00219691583784964, -5.514549477365426888, -3.283357778048667797 ) ) ;
#12916 = DIRECTION ( 'NONE',  ( 0.1113444980252557837, 0.9937818688019538493, -0.000000000000000000 ) ) ;
#12917 = DIRECTION ( 'NONE',  ( 0.000000000000000000, 0.000000000000000000, 1.000000000000000000 ) ) ;
#12918 = CARTESIAN_POINT ( 'NONE',  ( 33.46007730730551799, -5.886481946178435010, -4.705209693361169343 ) ) ;
#12919 = DIRECTION ( 'NONE',  ( 0.05980762113533198004, -0.4964101615137755941, 0.8660254037844384856 ) ) ;
#12920 = CARTESIAN_POINT ( 'NONE',  ( 29.30958546476020743, -4.505622649006972402, 3.283357778048664244 ) ) ;
#12921 = CARTESIAN_POINT ( 'NONE',  ( 31.03886041246737548, -3.043338102658604161, 7.939653947423664704 ) ) ;
#12922 = EDGE_CURVE ( 'NONE', #14411, #14109, #10449, .T. ) ;
#12923 = EDGE_LOOP ( 'NONE', ( #10008, #10418, #17699, #17957 ) ) ;
#12924 = ORIENTED_EDGE ( 'NONE', *, *, #8160, .T. ) ;
#12925 = CARTESIAN_POINT ( 'NONE',  ( 26.06962060539356330, -5.343074812781619443, 7.975991048337257361 ) ) ;
#12926 = EDGE_LOOP ( 'NONE', ( #6381, #2481, #13519, #11923 ) ) ;
#12927 = CARTESIAN_POINT ( 'NONE',  ( 26.25801688195511474, -3.619335333876111171, 3.627061608673666893 ) ) ;
#12928 = CARTESIAN_POINT ( 'NONE',  ( 31.78252145740879797, -2.026962321187214311, -4.533357778048659803 ) ) ;
#12929 = DIRECTION ( 'NONE',  ( 1.000000000000000000, 0.000000000000000000, 0.000000000000000000 ) ) ;
#12930 = ADVANCED_FACE ( 'NONE', ( #849 ), #6380, .F. ) ;
#12931 = ORIENTED_EDGE ( 'NONE', *, *, #106, .F. ) ;
#12932 = CARTESIAN_POINT ( 'NONE',  ( -25.11802603177690330, -19.03270077640483038, -0.5379818257722508434 ) ) ;
#12933 = DIRECTION ( 'NONE',  ( 0.1035898384862230237, -0.8598076211353317122, -0.5000000000000002220 ) ) ;
#12934 = DIRECTION ( 'NONE',  ( 0.000000000000000000, 0.000000000000000000, 1.000000000000000000 ) ) ;
#12935 = CARTESIAN_POINT ( 'NONE',  ( 26.14456121274580624, -5.685614013951941992, -8.283357778048664244 ) ) ;
#12936 = VECTOR ( 'NONE', #5170, 1000.000000000000000 ) ;
#12937 = ORIENTED_EDGE ( 'NONE', *, *, #3486, .F. ) ;
#12938 = CARTESIAN_POINT ( 'NONE',  ( 26.24741491880507027, -3.420740141806666745, -3.283357778048662023 ) ) ;
#12939 = CARTESIAN_POINT ( 'NONE',  ( 2.500000000000000000, 2.357898499370432166, -2.385244779468109755E-15 ) ) ;
#12940 = CARTESIAN_POINT ( 'NONE',  ( -5.384454397937117776, 6.594054843588580568E-16, -4.184454397937119374 ) ) ;
#12941 = CARTESIAN_POINT ( 'NONE',  ( 27.08121146544255353, -6.028038774645947839, -7.939653947423664704 ) ) ;
#12942 = ORIENTED_EDGE ( 'NONE', *, *, #3653, .T. ) ;
#12943 = CARTESIAN_POINT ( 'NONE',  ( 26.18940075748478691, -6.337263906362392341, -7.823530922983556124 ) ) ;
#12944 = CARTESIAN_POINT ( 'NONE',  ( 32.01903832059031174, -7.086814257134402162, 5.783357778048657138 ) ) ;
#12945 = EDGE_CURVE ( 'NONE', #17504, #9792, #16189, .T. ) ;
#12946 = EDGE_LOOP ( 'NONE', ( #17589, #12727, #8558, #5851 ) ) ;
#12947 = PRODUCT_DEFINITION_FORMATION_WITH_SPECIFIED_SOURCE ( 'ANY', '', #3615, .NOT_KNOWN. ) ;
#12948 = ORIENTED_EDGE ( 'NONE', *, *, #14036, .F. ) ;
#12949 = ORIENTED_EDGE ( 'NONE', *, *, #8746, .F. ) ;
#12950 = CARTESIAN_POINT ( 'NONE',  ( 26.92924972366625980, -7.310485091653801781, -5.783357778048657138 ) ) ;
#12951 = CARTESIAN_POINT ( 'NONE',  ( 35.41536221060850664, -16.03270077640482683, 0.5379818257722508434 ) ) ;
#12952 = EDGE_CURVE ( 'NONE', #11466, #3807, #8524, .T. ) ;
#12953 = DIRECTION ( 'NONE',  ( 1.000000000000000000, 0.000000000000000000, 0.000000000000000000 ) ) ;
#12954 = VECTOR ( 'NONE', #11711, 1000.000000000000000 ) ;
#12955 = CARTESIAN_POINT ( 'NONE',  ( 28.11132641904908169, -7.168068194032743534, 5.783357778048657138 ) ) ;
#12956 = DIRECTION ( 'NONE',  ( 0.8660254037844380415, 0.5000000000000008882, 0.000000000000000000 ) ) ;
#12957 = CARTESIAN_POINT ( 'NONE',  ( 31.87075164095941915, -4.197052703815608687, -3.627061608673664672 ) ) ;
#12958 = DIRECTION ( 'NONE',  ( -0.1196152422706611151, 0.9928203230275511881, 0.000000000000000000 ) ) ;
#12959 = DIRECTION ( 'NONE',  ( 0.9928203230275512992, 0.1196152422706610180, 4.006172263299093133E-17 ) ) ;
#12960 = CARTESIAN_POINT ( 'NONE',  ( 25.17121605730381972, -3.996982838752419553, 5.783357778048662468 ) ) ;
#12961 = CARTESIAN_POINT ( 'NONE',  ( 1.500000000000000000, 11.00000000000000000, -3.000000000000000000 ) ) ;
#12962 = PRODUCT_DEFINITION_CONTEXT ( 'detailed design', #11649, 'design' ) ;
#12963 = DIRECTION ( 'NONE',  ( -5.026720092345836698E-22, 4.581671729415424240E-22, -1.000000000000000000 ) ) ;
#12964 = ORIENTED_EDGE ( 'NONE', *, *, #3490, .F. ) ;
#12965 = CARTESIAN_POINT ( 'NONE',  ( 28.36401332423200827, -6.500457016816879374, -6.861505862736166250 ) ) ;
#12966 = CARTESIAN_POINT ( 'NONE',  ( 30.52163964716380917, -2.178873678870954400, -4.533357778048659803 ) ) ;
#12967 = FACE_OUTER_BOUND ( 'NONE', #17101, .T. ) ;
#12968 = CARTESIAN_POINT ( 'NONE',  ( 4.198928548860774157, -0.8158838809860105012, -3.226471437616921012 ) ) ;
#12969 = VERTEX_POINT ( 'NONE', #12075 ) ;
#12970 = CARTESIAN_POINT ( 'NONE',  ( -7.511572993685817836E-16, -4.618802153517020059, -3.133295621305386636 ) ) ;
#12971 = AXIS2_PLACEMENT_3D ( 'NONE', #6263, #2017, #13338 ) ;
#12972 = ADVANCED_FACE ( 'NONE', ( #14900 ), #5184, .T. ) ;
#12973 = CARTESIAN_POINT ( 'NONE',  ( 29.23078034989804763, -4.515117109069654688, 3.283357778048664244 ) ) ;
#12974 = ORIENTED_EDGE ( 'NONE', *, *, #3204, .T. ) ;
#12975 = VECTOR ( 'NONE', #8618, 1000.000000000000000 ) ;
#12976 = CARTESIAN_POINT ( 'NONE',  ( 31.93198502805756789, -2.935734224299280548, -7.939653947423660263 ) ) ;
#12977 = EDGE_LOOP ( 'NONE', ( #10892, #16891 ) ) ;
#12978 = CARTESIAN_POINT ( 'NONE',  ( 29.15568435273173264, -2.343444316361667834, -7.033357778048658027 ) ) ;
#12979 = PLANE ( 'NONE',  #11875 ) ;
#12980 = AXIS2_PLACEMENT_3D ( 'NONE', #16143, #14775, #4786 ) ;
#12981 = CARTESIAN_POINT ( 'NONE',  ( 28.52162355051263987, -6.481468097106410475, -6.861505862736167138 ) ) ;
#12982 = EDGE_CURVE ( 'NONE', #9800, #13928, #16276, .T. ) ;
#12983 = VECTOR ( 'NONE', #16977, 1000.000000000000000 ) ;
#12984 = CARTESIAN_POINT ( 'NONE',  ( 26.31556265977298992, -7.384422263489805793, 5.783357778048663356 ) ) ;
#12985 = CARTESIAN_POINT ( 'NONE',  ( 27.93049598394382116, -4.671775696577297410, -3.627061608673664672 ) ) ;
#12986 = DIRECTION ( 'NONE',  ( 0.000000000000000000, 0.000000000000000000, 1.000000000000000000 ) ) ;
#12987 = CARTESIAN_POINT ( 'NONE',  ( 32.84384354600314282, -1.561735352540135180, -6.453230759126467042 ) ) ;
#12988 = CARTESIAN_POINT ( 'NONE',  ( 27.16987539990068612, -2.245336462116964249, 5.113484796970861446 ) ) ;
#12989 = CARTESIAN_POINT ( 'NONE',  ( 30.04891049036066164, -7.324175753722694360, -5.783357778048669573 ) ) ;
#12990 = DIRECTION ( 'NONE',  ( -0.000000000000000000, -0.000000000000000000, -1.000000000000000000 ) ) ;
#12991 = CARTESIAN_POINT ( 'NONE',  ( 25.37303892199676270, -2.799178389412888546, 4.533357778048667797 ) ) ;
#12992 = AXIS2_PLACEMENT_3D ( 'NONE', #9720, #2853, #6669 ) ;
#12993 = ORIENTED_EDGE ( 'NONE', *, *, #10180, .T. ) ;
#12994 = DIRECTION ( 'NONE',  ( 0.000000000000000000, 0.000000000000000000, 1.000000000000000000 ) ) ;
#12995 = CARTESIAN_POINT ( 'NONE',  ( 25.74999999999998934, -16.21813761408365195, -13.00000000000000355 ) ) ;
#12996 = PLANE ( 'NONE',  #3741 ) ;
#12997 = ORIENTED_EDGE ( 'NONE', *, *, #8405, .F. ) ;
#12998 = DIRECTION ( 'NONE',  ( 0.9928203230275510771, 0.1196152422706609902, 4.006172263299092517E-17 ) ) ;
#12999 = AXIS2_PLACEMENT_3D ( 'NONE', #11166, #16737, #8482 ) ;
#13000 = VERTEX_POINT ( 'NONE', #16837 ) ;
#13001 = CARTESIAN_POINT ( 'NONE',  ( 3.538288549924106796, -15.34800872113743431, -16.99955934415557479 ) ) ;
#13002 = CARTESIAN_POINT ( 'NONE',  ( 26.01595305975170547, -2.384361315936983416, 5.783357778048657138 ) ) ;
#13003 = EDGE_CURVE ( 'NONE', #2915, #17680, #15550, .T. ) ;
#13004 = EDGE_CURVE ( 'NONE', #7158, #11222, #14090, .T. ) ;
#13005 = VECTOR ( 'NONE', #16636, 1000.000000000000000 ) ;
#13006 = CARTESIAN_POINT ( 'NONE',  ( 30.61929490284659394, -6.528548903775525325, -4.533357778048668685 ) ) ;
#13007 = DIRECTION ( 'NONE',  ( -0.1196152422706610735, 0.9928203230275511881, 0.000000000000000000 ) ) ;
#13008 = CONTEXT_DEPENDENT_SHAPE_REPRESENTATION ( #7614, #13602 ) ;
#13009 = CARTESIAN_POINT ( 'NONE',  ( 7.499998387031003411, -20.49508120620799900, -12.00000000000000000 ) ) ;
#13010 = CARTESIAN_POINT ( 'NONE',  ( 8.776279441628840772, 6.799038105676637578, -2.000000000000000000 ) ) ;
#13011 = CARTESIAN_POINT ( 'NONE',  ( 0.000000000000000000, 0.000000000000000000, -10.00000000000000000 ) ) ;
#13012 = DIRECTION ( 'NONE',  ( 1.000000000000000000, 0.000000000000000000, 0.000000000000000000 ) ) ;
#13013 = CARTESIAN_POINT ( 'NONE',  ( 27.88665588685489993, -3.423116496867954162, 7.939653947423664704 ) ) ;
#13014 = VERTEX_POINT ( 'NONE', #5745 ) ;
#13015 = AXIS2_PLACEMENT_3D ( 'NONE', #11900, #17483, #10535 ) ;
#13016 = CARTESIAN_POINT ( 'NONE',  ( 39.22222685913116180, -5.829424113971213295, -5.783357778048662468 ) ) ;
#13017 = ORIENTED_EDGE ( 'NONE', *, *, #1913, .T. ) ;
#13018 = CARTESIAN_POINT ( 'NONE',  ( 33.32855701603872234, -2.140504347050403045, 4.705209693361168455 ) ) ;
#13019 = CARTESIAN_POINT ( 'NONE',  ( -23.83446850436624587, -10.01089291621719646, 14.74374009921848483 ) ) ;
#13020 = CARTESIAN_POINT ( 'NONE',  ( 27.18555652250208610, -2.580805812949960920, -7.033357778048658027 ) ) ;
#13021 = EDGE_LOOP ( 'NONE', ( #13528, #7064, #2463, #7564 ) ) ;
#13022 = CARTESIAN_POINT ( 'NONE',  ( -3.248936832696171617, -15.16081378324841111, -17.00000000000000000 ) ) ;
#13023 = DIRECTION ( 'NONE',  ( -0.000000000000000000, -0.000000000000000000, 1.000000000000000000 ) ) ;
#13024 = EDGE_CURVE ( 'NONE', #5360, #2932, #8163, .T. ) ;
#13025 = CARTESIAN_POINT ( 'NONE',  ( 25.29083129957448151, -4.989803161779970964, -5.783357778048664244 ) ) ;
#13026 = DIRECTION ( 'NONE',  ( -1.000000000000000000, 0.000000000000000000, 0.000000000000000000 ) ) ;
#13028 = EDGE_CURVE ( 'NONE', #6811, #3520, #9110, .T. ) ;
#13027 = CARTESIAN_POINT ( 'NONE',  ( 26.00347982711925710, -2.723222710571018279, -7.033357778048658027 ) ) ;
#13029 = CARTESIAN_POINT ( 'NONE',  ( 27.27683486999669427, -2.232449958253242883, 5.783357778048667797 ) ) ;
#13030 = CARTESIAN_POINT ( 'NONE',  ( 3.443595183066687326, -15.28297513750540837, 16.99984776326510172 ) ) ;
#13031 = CARTESIAN_POINT ( 'NONE',  ( 26.34117031759772942, -2.982346454214467535, -4.705209693361161349 ) ) ;
#13032 = ORIENTED_EDGE ( 'NONE', *, *, #106, .T. ) ;
#13033 = CIRCLE ( 'NONE', #585, 5.000000000000000000 ) ;
#13034 = ADVANCED_FACE ( 'NONE', ( #4575 ), #5278, .T. ) ;
#13035 = CARTESIAN_POINT ( 'NONE',  ( 26.08205926866327218, -5.446317154234562530, -8.158109112226842541 ) ) ;
#13036 = CARTESIAN_POINT ( 'NONE',  ( 31.83134908525019213, -4.201799933639492224, 3.283357778048664244 ) ) ;
#13037 = ORIENTED_EDGE ( 'NONE', *, *, #1345, .T. ) ;
#13038 = EDGE_LOOP ( 'NONE', ( #3076, #17598, #10354, #12931 ) ) ;
#13039 = VECTOR ( 'NONE', #11164, 1000.000000000000000 ) ;
#13040 = ORIENTED_EDGE ( 'NONE', *, *, #8255, .F. ) ;
#13041 = ORIENTED_EDGE ( 'NONE', *, *, #6436, .T. ) ;
#13042 = CARTESIAN_POINT ( 'NONE',  ( 27.12505156253147831, -7.276697974355292864, 5.783357778048658915 ) ) ;
#13043 = CARTESIAN_POINT ( 'NONE',  ( -8.812506826975363694, -18.97024042328638416, -16.83711976780714181 ) ) ;
#13044 = CARTESIAN_POINT ( 'NONE',  ( -3.248936832696171617, 17.78798921770683350, -17.00000000000000000 ) ) ;
#13045 = CARTESIAN_POINT ( 'NONE',  ( -2.749999999999992895, -20.49999999999999645, 6.000000000000000000 ) ) ;
#13046 = CARTESIAN_POINT ( 'NONE',  ( -17.08586189024356727, -18.24992599651649527, -15.98693133205340189 ) ) ;
#13047 = CARTESIAN_POINT ( 'NONE',  ( 32.81641299864316608, -4.083119185552795294, -7.939653947423662039 ) ) ;
#13048 = CARTESIAN_POINT ( 'NONE',  ( -7.499998387031003411, -20.49508120620799900, -13.00000000000000178 ) ) ;
#13049 = DIRECTION ( 'NONE',  ( 0.8660254037844397068, 0.4999999999999981126, -0.000000000000000000 ) ) ;
#13050 = ORIENTED_EDGE ( 'NONE', *, *, #10386, .F. ) ;
#13052 = ADVANCED_FACE ( 'NONE', ( #2559 ), #11916, .F. ) ;
#13051 = DIRECTION ( 'NONE',  ( 0.000000000000000000, 0.000000000000000000, -1.000000000000000000 ) ) ;
#13053 = CARTESIAN_POINT ( 'NONE',  ( 5.000000000000004441, 5.204748896376250699E-16, -4.250000000000000000 ) ) ;
#13054 = CIRCLE ( 'NONE', #2372, 5.000000000000000000 ) ;
#13055 = CARTESIAN_POINT ( 'NONE',  ( 25.71748644841968456, -2.420320648352046078, 5.783357778048663356 ) ) ;
#13056 = ORIENTED_EDGE ( 'NONE', *, *, #9691, .T. ) ;
#13057 = AXIS2_PLACEMENT_3D ( 'NONE', #3276, #1835, #3175 ) ;
#13058 = CARTESIAN_POINT ( 'NONE',  ( 28.10549950023366961, -2.142809097641162897, -5.783357778048658027 ) ) ;
#13059 = CARTESIAN_POINT ( 'NONE',  ( 0.000000000000000000, 0.000000000000000000, -10.50000000000000000 ) ) ;
#13060 = ORIENTED_EDGE ( 'NONE', *, *, #9985, .F. ) ;
#13061 = EDGE_CURVE ( 'NONE', #6735, #6225, #2663, .T. ) ;
#13062 = CARTESIAN_POINT ( 'NONE',  ( 2.171643655288375996, -3.365003104552331870, -9.156896733678572738E-15 ) ) ;
#13063 = VECTOR ( 'NONE', #13049, 1000.000000000000000 ) ;
#13064 = CARTESIAN_POINT ( 'NONE',  ( 26.79905070906540132, -3.354278923027479209, 8.283357778048664244 ) ) ;
#13065 = ORIENTED_EDGE ( 'NONE', *, *, #2887, .T. ) ;
#13066 = DIRECTION ( 'NONE',  ( 0.9928203230275512992, 0.1196152422706614898, -0.000000000000000000 ) ) ;
#13067 = AXIS2_PLACEMENT_3D ( 'NONE', #11706, #3378, #1942 ) ;
#13068 = CARTESIAN_POINT ( 'NONE',  ( 32.56242593318006584, -2.859778545457409837, -7.939653947423660263 ) ) ;
#13069 = VERTEX_POINT ( 'NONE', #16437 ) ;
#13070 = CARTESIAN_POINT ( 'NONE',  ( 30.00264913441657555, -6.940201157507134511, -5.783357778048657138 ) ) ;
#13071 = CARTESIAN_POINT ( 'NONE',  ( 25.96814307759224150, -4.500799614243312874, -8.119953194407841579 ) ) ;
#13072 = EDGE_LOOP ( 'NONE', ( #4983, #13890, #15268, #5683, #12638 ) ) ;
#13073 = VECTOR ( 'NONE', #9658, 1000.000000000000000 ) ;
#13074 = EDGE_CURVE ( 'NONE', #17574, #1161, #10957, .T. ) ;
#13075 = CARTESIAN_POINT ( 'NONE',  ( -4.000000000000000000, 2.309401076758501592, -3.133295621305381307 ) ) ;
#13076 = CARTESIAN_POINT ( 'NONE',  ( 26.46816385032927599, -3.594016774262162706, -3.627061608673662896 ) ) ;
#13077 = VECTOR ( 'NONE', #16008, 999.9999999999998863 ) ;
#13078 = CYLINDRICAL_SURFACE ( 'NONE', #6406, 2.499999999999999112 ) ;
#13079 = CARTESIAN_POINT ( 'NONE',  ( 33.15485366002904755, -6.560422763297783177, -5.783357778048663356 ) ) ;
#13080 = FACE_OUTER_BOUND ( 'NONE', #15235, .T. ) ;
#13081 = AXIS2_PLACEMENT_3D ( 'NONE', #1558, #13874, #12519 ) ;
#13082 = ORIENTED_EDGE ( 'NONE', *, *, #992, .T. ) ;
#13083 = CARTESIAN_POINT ( 'NONE',  ( 27.81599742762458050, -2.504850134108091098, -7.033357778048658027 ) ) ;
#13084 = CARTESIAN_POINT ( 'NONE',  ( -25.11802603177690330, -16.03270077640482683, -10.53798182577225084 ) ) ;
#13085 = VECTOR ( 'NONE', #614, 1000.000000000000000 ) ;
#13086 = EDGE_LOOP ( 'NONE', ( #17449, #10927, #3733, #17823, #15162 ) ) ;
#13087 = CARTESIAN_POINT ( 'NONE',  ( 31.39792096211754924, -4.254019462947003838, 3.627061608673664228 ) ) ;
#13088 = B_SPLINE_CURVE_WITH_KNOTS ( 'NONE', 3,
 ( #413, #4825, #3391, #13184, #6198, #11719 ),
 .UNSPECIFIED., .F., .F.,
 ( 4, 2, 4 ),
 ( 0.8480943072472125754, 0.9070911586903380730, 0.9660880101334634595 ),
 .UNSPECIFIED. ) ;
#13089 = EDGE_CURVE ( 'NONE', #7189, #13433, #2650, .T. ) ;
#13090 = VERTEX_POINT ( 'NONE', #1204 ) ;
#13091 = CARTESIAN_POINT ( 'NONE',  ( 30.72436838703367812, -6.515889623968540434, -7.033357778048666908 ) ) ;
#13092 = CARTESIAN_POINT ( 'NONE',  ( -23.47400307746860548, -29.47066586337336247, -14.90105725137467552 ) ) ;
#13093 = CARTESIAN_POINT ( 'NONE',  ( 34.91600907648203389, -11.88801210197604341, -11.56671555609732671 ) ) ;
#13094 = ORIENTED_EDGE ( 'NONE', *, *, #8746, .T. ) ;
#13095 = CARTESIAN_POINT ( 'NONE',  ( 26.21973641492267859, -6.589053366008232437, -7.643209271886766132 ) ) ;
#13096 = DIRECTION ( 'NONE',  ( 1.000000000000000000, 0.000000000000000000, 0.000000000000000000 ) ) ;
#13097 = CARTESIAN_POINT ( 'NONE',  ( 25.92409770820621162, -4.135217962343409326, -3.765474553462066165 ) ) ;
#13098 = EDGE_CURVE ( 'NONE', #11309, #11700, #6817, .T. ) ;
#13099 = CARTESIAN_POINT ( 'NONE',  ( 26.31556265977298992, -7.384422263489805793, 5.783357778048663356 ) ) ;
#13100 = CARTESIAN_POINT ( 'NONE',  ( -9.750000000000035527, -3.897114317029883868, -3.000000000000002665 ) ) ;
#13101 = VECTOR ( 'NONE', #15104, 1000.000000000000114 ) ;
#13102 = AXIS2_PLACEMENT_3D ( 'NONE', #5087, #9351, #11984 ) ;
#13103 = CARTESIAN_POINT ( 'NONE',  ( 29.78612525785423060, -2.267488637519798012, -7.033357778048658027 ) ) ;
#13104 = CARTESIAN_POINT ( 'NONE',  ( 25.11802603177690330, -19.03270077640483038, -0.5379818257722508434 ) ) ;
#13105 = CONTEXT_DEPENDENT_SHAPE_REPRESENTATION ( #8532, #13458 ) ;
#13106 = DIRECTION ( 'NONE',  ( -0.000000000000000000, -0.000000000000000000, -1.000000000000000000 ) ) ;
#13107 = CARTESIAN_POINT ( 'NONE',  ( 31.56875459193803124, -6.114348982704044921, -4.705209693361169343 ) ) ;
#13108 = DIRECTION ( 'NONE',  ( 1.000000000000000000, 0.000000000000000000, 0.000000000000000000 ) ) ;
#13109 = CARTESIAN_POINT ( 'NONE',  ( -5.499998817156067865, -20.49639288455253450, 12.00000000000000000 ) ) ;
#13110 = CARTESIAN_POINT ( 'NONE',  ( 26.01127209431523113, -6.877383572197488526, 4.531664423152620635 ) ) ;
#13111 = ADVANCED_FACE ( 'NONE', ( #13533 ), #11524, .F. ) ;
#13112 = EDGE_LOOP ( 'NONE', ( #2749, #13474, #7197, #986 ) ) ;
#13113 = CARTESIAN_POINT ( 'NONE',  ( 26.45077056032005913, -6.103994453487816330, -7.939653947423664704 ) ) ;
#13114 = ORIENTED_EDGE ( 'NONE', *, *, #3823, .F. ) ;
#13115 = CARTESIAN_POINT ( 'NONE',  ( 32.07220196432897552, -5.426722983814484813, 7.939653947423658487 ) ) ;
#13116 = CARTESIAN_POINT ( 'NONE',  ( 0.000000000000000000, 0.000000000000000000, -3.000000000000000000 ) ) ;
#13117 = DIRECTION ( 'NONE',  ( 0.8660254037844432595, 0.4999999999999921174, 0.000000000000000000 ) ) ;
#13118 = ORIENTED_EDGE ( 'NONE', *, *, #8317, .F. ) ;
#13119 = CARTESIAN_POINT ( 'NONE',  ( 27.82847066025702887, -2.165988739474055791, -5.783357778048658027 ) ) ;
#13120 = PLANE ( 'NONE',  #17104 ) ;
#13121 = VERTEX_POINT ( 'NONE', #6719 ) ;
#13122 = CARTESIAN_POINT ( 'NONE',  ( 27.87912141988533676, -2.159886323212414361, -6.453230759126469707 ) ) ;
#13123 = EDGE_CURVE ( 'NONE', #13121, #16345, #2741, .T. ) ;
#13124 = CARTESIAN_POINT ( 'NONE',  ( 8.409399735147211686E-16, 4.618802153517009401, -3.133295621305383083 ) ) ;
#13125 = CARTESIAN_POINT ( 'NONE',  ( 26.47260139170898441, -4.847423203795396596, -3.283357778048664688 ) ) ;
#13126 = DIRECTION ( 'NONE',  ( 0.000000000000000000, -1.287488025362403787E-15, -1.000000000000000000 ) ) ;
#13127 = DIRECTION ( 'NONE',  ( 0.000000000000000000, -0.5027044994213123452, 0.8644583195629317318 ) ) ;
#13128 =( NAMED_UNIT ( * ) SI_UNIT ( $, .STERADIAN. ) SOLID_ANGLE_UNIT ( ) );
#13129 = CARTESIAN_POINT ( 'NONE',  ( 29.50659824675005893, -4.481886499472614638, -7.939653947423662039 ) ) ;
#13130 = VERTEX_POINT ( 'NONE', #9690 ) ;
#13131 = LINE ( 'NONE', #6233, #610 ) ;
#13132 = CARTESIAN_POINT ( 'NONE',  ( 30.88568772756644520, -4.315733451902305617, 8.283357778048662468 ) ) ;
#13133 = ADVANCED_FACE ( 'NONE', ( #6899 ), #2397, .F. ) ;
#13134 = EDGE_LOOP ( 'NONE', ( #9597, #4656, #13135, #11849, #4629 ) ) ;
#13135 = ORIENTED_EDGE ( 'NONE', *, *, #11460, .T. ) ;
#13136 = ORIENTED_EDGE ( 'NONE', *, *, #1038, .F. ) ;
#13137 = CARTESIAN_POINT ( 'NONE',  ( 27.38828526237195504, -6.917821758047558056, 7.033357778048657138 ) ) ;
#13138 = FACE_OUTER_BOUND ( 'NONE', #8573, .T. ) ;
#13139 = CARTESIAN_POINT ( 'NONE',  ( 19.71718888926881164, -28.93397812220195675, -15.64003640126281347 ) ) ;
#13140 = CARTESIAN_POINT ( 'NONE',  ( 29.16815758536418102, -2.004582921727632971, -5.783357778048664244 ) ) ;
#13141 = CARTESIAN_POINT ( 'NONE',  ( -19.71718888926883650, -28.93397812220196030, 15.64003640126278682 ) ) ;
#13142 = CARTESIAN_POINT ( 'NONE',  ( 32.69811611091622439, -2.216460025892273311, -6.861505862736158257 ) ) ;
#13143 = DIRECTION ( 'NONE',  ( 0.9928203230275512992, 0.1196152422706614482, 0.000000000000000000 ) ) ;
#13144 = LINE ( 'NONE', #14333, #17134 ) ;
#13145 = VERTEX_POINT ( 'NONE', #12612 ) ;
#13146 = CARTESIAN_POINT ( 'NONE',  ( -1.747541505913278614, 3.837784562140256650, -3.203702292528908924 ) ) ;
#13147 = CARTESIAN_POINT ( 'NONE',  ( 9.749999999999982236, -3.897114317030018871, -3.000000000000000000 ) ) ;
#13148 = CARTESIAN_POINT ( 'NONE',  ( 21.03312194624853149, -10.28219102306256971, 15.32075016948875934 ) ) ;
#13149 = ORIENTED_EDGE ( 'NONE', *, *, #557, .F. ) ;
#13150 = CIRCLE ( 'NONE', #15177, 5.500000000000000000 ) ;
#13151 = CARTESIAN_POINT ( 'NONE',  ( 27.75549246765397271, -7.200742295513423485, -5.783357778048668685 ) ) ;
#13152 = CARTESIAN_POINT ( 'NONE',  ( 32.30426898124760982, -6.025734024055190652, -6.861505862736167138 ) ) ;
#13153 = ORIENTED_EDGE ( 'NONE', *, *, #3475, .T. ) ;
#13154 = DIRECTION ( 'NONE',  ( -0.1414213562373112243, -0.9899494936611663576, 0.000000000000000000 ) ) ;
#13155 = CARTESIAN_POINT ( 'NONE',  ( 29.14074637024071635, -5.979778010479330774, 8.283357778048658915 ) ) ;
#13156 = PRODUCT_DEFINITION_SHAPE ( 'NONE', 'NONE',  #17983 ) ;
#13157 = ADVANCED_FACE ( 'NONE', ( #15239 ), #470, .T. ) ;
#13158 = ORIENTED_EDGE ( 'NONE', *, *, #17416, .F. ) ;
#13159 = CARTESIAN_POINT ( 'NONE',  ( 4.000000000000000000, 0.3987449864459997606, -0.01220643443059902904 ) ) ;
#13160 = ORIENTED_EDGE ( 'NONE', *, *, #15391, .T. ) ;
#13161 = CARTESIAN_POINT ( 'NONE',  ( 32.34358231980129261, -4.140085944684206432, -3.627061608673664672 ) ) ;
#13162 = ORIENTED_EDGE ( 'NONE', *, *, #5854, .F. ) ;
#13163 = CARTESIAN_POINT ( 'NONE',  ( 33.00465954875439678, 3.976409685033599484, 3.995355914169179040E-15 ) ) ;
#13164 = CARTESIAN_POINT ( 'NONE',  ( 33.50243880635947846, -1.482387629897225390, -5.783357778048663356 ) ) ;
#13165 = EDGE_CURVE ( 'NONE', #8339, #17201, #17728, .T. ) ;
#13166 = CARTESIAN_POINT ( 'NONE',  ( 27.27683486999669427, -2.232449958253242883, -5.783357778048658027 ) ) ;
#13167 =( BOUNDED_CURVE ( )  B_SPLINE_CURVE ( 2, ( #17542, #17083, #15801, #3194, #12896, #4638, #8822, #14784, #3810 ),
 .UNSPECIFIED., .F., .T. ) 
 B_SPLINE_CURVE_WITH_KNOTS ( ( 3, 2, 2, 2, 3 ),
 ( 0.8653846153846154188, 0.8717948717948718063, 0.8846153846153845812, 0.8974358974358974672, 0.9038461538461538547 ),
 .UNSPECIFIED. ) 
 CURVE ( )  GEOMETRIC_REPRESENTATION_ITEM ( )  RATIONAL_B_SPLINE_CURVE ( ( 0.9330127018922192983, 0.9330127018922198534, 1.000000000000000000, 0.8660254037844387076, 1.000000000000000000, 0.8660254037844387076, 1.000000000000000000, 0.9330127018922194093, 0.9330127018922194093 ) ) 
 REPRESENTATION_ITEM ( '' )  );
#13168 = CARTESIAN_POINT ( 'NONE',  ( -0.1750032273043209963, -4.719840313910222740, -3.169254239516217986 ) ) ;
#13169 = CARTESIAN_POINT ( 'NONE',  ( 27.63266882139180680, -2.199775856772564708, -5.783357778048658027 ) ) ;
#13170 = ORIENTED_EDGE ( 'NONE', *, *, #8391, .F. ) ;
#13171 = CARTESIAN_POINT ( 'NONE',  ( -36.27615609941022257, -23.17738945083361557, 12.00000000000000000 ) ) ;
#13172 = CARTESIAN_POINT ( 'NONE',  ( -2.016448651773435938E-27, -20.49999999999999645, -6.000000000000000000 ) ) ;
#13173 = CARTESIAN_POINT ( 'NONE',  ( 25.71748644841968456, -2.420320648352046078, 5.783357778048663356 ) ) ;
#13174 = CARTESIAN_POINT ( 'NONE',  ( 25.90934487712385348, 0.1208734971681838660, -5.783357778048663356 ) ) ;
#13175 = CARTESIAN_POINT ( 'NONE',  ( 27.96989853965305528, -4.667028466753395222, -8.283357778048662468 ) ) ;
#13176 = FACE_OUTER_BOUND ( 'NONE', #3927, .T. ) ;
#13177 = EDGE_CURVE ( 'NONE', #14372, #15406, #13272, .T. ) ;
#13178 = EDGE_LOOP ( 'NONE', ( #1564, #12551, #10492, #13734, #3621, #2869 ) ) ;
#13179 = LINE ( 'NONE', #11803, #1982 ) ;
#13180 = DIRECTION ( 'NONE',  ( -1.000000000000000000, 0.000000000000000000, 0.000000000000000000 ) ) ;
#13181 = CYLINDRICAL_SURFACE ( 'NONE', #11833, 2.500000000000001776 ) ;
#13182 = ADVANCED_FACE ( 'NONE', ( #11218 ), #12884, .T. ) ;
#13183 = EDGE_LOOP ( 'NONE', ( #9927, #223, #1657, #13477 ) ) ;
#13184 = CARTESIAN_POINT ( 'NONE',  ( 26.28640587110349713, -7.142417550747740762, 4.663187713370804843 ) ) ;
#13185 = DIRECTION ( 'NONE',  ( 1.000000000000000000, 0.000000000000000000, 0.000000000000000000 ) ) ;
#13186 = FACE_BOUND ( 'NONE', #11109, .T. ) ;
#13187 = CARTESIAN_POINT ( 'NONE',  ( 32.32618902979206865, -6.650063623909865385, -5.783357778048669573 ) ) ;
#13188 = CARTESIAN_POINT ( 'NONE',  ( 29.77044413525282707, -1.932019286686802895, 5.113484796970859669 ) ) ;
#13189 = EDGE_CURVE ( 'NONE', #17076, #8674, #3179, .T. ) ;
#13190 = CARTESIAN_POINT ( 'NONE',  ( 28.49145532429760053, -1.696564004353941613, -5.783357778048658027 ) ) ;
#13191 = FACE_OUTER_BOUND ( 'NONE', #1902, .T. ) ;
#13192 = DIRECTION ( 'NONE',  ( -1.000000000000000000, -0.000000000000000000, -0.000000000000000000 ) ) ;
#13193 = CARTESIAN_POINT ( 'NONE',  ( -45.50000000000000000, -19.03270077640483038, 5.537981825772250843 ) ) ;
#13194 = CARTESIAN_POINT ( 'NONE',  ( 29.66420847303068697, -4.462897579762144851, -7.939653947423662039 ) ) ;
#13195 = LINE ( 'NONE', #10279, #13980 ) ;
#13196 = AXIS2_PLACEMENT_3D ( 'NONE', #5385, #15101, #10819 ) ;
#13197 = CARTESIAN_POINT ( 'NONE',  ( 31.86581749455020329, -6.715726164782562790, -5.113484796970860558 ) ) ;
#13198 = CARTESIAN_POINT ( 'NONE',  ( 27.28266178881210280, -7.257709054644824853, 5.783357778048657138 ) ) ;
#13199 = EDGE_CURVE ( 'NONE', #6265, #227, #7778, .T. ) ;
#13200 = EDGE_LOOP ( 'NONE', ( #6473, #15359, #2989, #17953 ) ) ;
#13201 = CARTESIAN_POINT ( 'NONE',  ( 26.19644603989336318, -6.395740563884610097, 7.560328637605171487 ) ) ;
#13202 = ORIENTED_EDGE ( 'NONE', *, *, #9983, .T. ) ;
#13203 = CARTESIAN_POINT ( 'NONE',  ( 32.91278983782564183, -5.325448745358647429, 3.627061608673662896 ) ) ;
#13204 = DIRECTION ( 'NONE',  ( 0.000000000000000000, 0.000000000000000000, 1.000000000000000000 ) ) ;
#13205 = DIRECTION ( 'NONE',  ( 0.9396926207859143121, 1.150791560227857665E-16, -0.3420201433256525592 ) ) ;
#13206 = ORIENTED_EDGE ( 'NONE', *, *, #16971, .F. ) ;
#13207 = DIRECTION ( 'NONE',  ( -1.000000000000000000, 0.000000000000000000, 0.000000000000000000 ) ) ;
#13208 = CARTESIAN_POINT ( 'NONE',  ( 30.37154917142620292, -2.923863409590206519, 3.283357778048666464 ) ) ;
#13209 = VERTEX_POINT ( 'NONE', #2906 ) ;
#13210 = DIRECTION ( 'NONE',  ( -0.9928203230275512992, -0.1196152422706610180, -4.006172263299093133E-17 ) ) ;
#13211 = DIRECTION ( 'NONE',  ( -0.1196152422706597551, 0.9928203230275514102, 0.000000000000000000 ) ) ;
#13212 = CARTESIAN_POINT ( 'NONE',  ( 32.34358231980129261, -4.140085944684206432, -3.627061608673664672 ) ) ;
#13213 = EDGE_CURVE ( 'NONE', #16314, #8286, #7094, .T. ) ;
#13214 = CARTESIAN_POINT ( 'NONE',  ( 0.1750032273043211906, 4.719840313910212082, -3.169254239516213989 ) ) ;
#13215 = DIRECTION ( 'NONE',  ( -0.000000000000000000, -0.000000000000000000, -1.000000000000000000 ) ) ;
#13216 = SHAPE_REPRESENTATION_RELATIONSHIP ( 'NONE' , 'NONE' ,  #691, #755 ) ;
#13217 = CARTESIAN_POINT ( 'NONE',  ( 28.87615734162756453, -4.557842178314484016, -7.939653947423662039 ) ) ;
#13218 = CARTESIAN_POINT ( 'NONE',  ( 31.63927044622584717, -1.706862622621797110, -5.113484796970854340 ) ) ;
#13219 = CARTESIAN_POINT ( 'NONE',  ( 33.27992013083530054, -6.934902899450660740, 5.783357778048657138 ) ) ;
#13220 = VERTEX_POINT ( 'NONE', #5701 ) ;
#13221 = ORIENTED_EDGE ( 'NONE', *, *, #13991, .F. ) ;
#13222 = ORIENTED_EDGE ( 'NONE', *, *, #8234, .F. ) ;
#13223 = CARTESIAN_POINT ( 'NONE',  ( 27.08121146544255353, -6.028038774645947839, 3.627061608673662896 ) ) ;
#13224 = CARTESIAN_POINT ( 'NONE',  ( 33.56515079149260572, -5.873822666371450119, 4.705209693361159573 ) ) ;
#13225 = PRESENTATION_STYLE_ASSIGNMENT (( #7699 ) ) ;
#13226 = CARTESIAN_POINT ( 'NONE',  ( 29.46348657678868577, -6.667800981652280967, -7.033357778048666908 ) ) ;
#13227 = DIRECTION ( 'NONE',  ( 0.5000000000000009992, -0.8660254037844381525, 0.000000000000000000 ) ) ;
#13228 = CARTESIAN_POINT ( 'NONE',  ( 30.93831368681553684, -6.190304661545915188, -4.705209693361169343 ) ) ;
#13229 = CARTESIAN_POINT ( 'NONE',  ( 29.23078034989804763, -4.515117109069654688, 3.283357778048664244 ) ) ;
#13230 = DIRECTION ( 'NONE',  ( -0.7866107318554605987, 0.6174492339697383869, 8.659560562354860135E-17 ) ) ;
#13231 = CARTESIAN_POINT ( 'NONE',  ( 32.30788887834420819, -1.963665922152317833, -7.033357778048658027 ) ) ;
#13232 = CARTESIAN_POINT ( 'NONE',  ( 31.37049041475757605, -6.775403295959669947, -6.453230759126470595 ) ) ;
#13233 = EDGE_CURVE ( 'NONE', #9792, #17313, #4625, .T. ) ;
#13234 = CARTESIAN_POINT ( 'NONE',  ( 16.79147592569384173, -15.38964587861223166, 16.02981638571824163 ) ) ;
#13235 = EDGE_CURVE ( 'NONE', #11222, #8791, #12788, .T. ) ;
#13236 = CARTESIAN_POINT ( 'NONE',  ( 26.49461065740898036, -7.352653653197164019, -5.783357778048668685 ) ) ;
#13237 = CARTESIAN_POINT ( 'NONE',  ( 30.80679339554874119, -2.444327062417882779, -6.861505862736158257 ) ) ;
#13238 = ORIENTED_EDGE ( 'NONE', *, *, #11942, .T. ) ;
#13239 = CARTESIAN_POINT ( 'NONE',  ( 20.25000000000000355, -16.21813761408365195, 0.000000000000000000 ) ) ;
#13240 = CARTESIAN_POINT ( 'NONE',  ( 33.15485366002904755, -6.560422763297783177, 5.783357778048664244 ) ) ;
#13241 = VECTOR ( 'NONE', #11146, 1000.000000000000114 ) ;
#13242 = ORIENTED_EDGE ( 'NONE', *, *, #8118, .F. ) ;
#13243 = DIRECTION ( 'NONE',  ( -0.1196152422706611984, 0.9928203230275510771, 0.000000000000000000 ) ) ;
#13244 = CARTESIAN_POINT ( 'NONE',  ( 32.14665875496697822, -6.044722943765660439, -6.861505862736166250 ) ) ;
#13245 = ORIENTED_EDGE ( 'NONE', *, *, #14935, .F. ) ;
#13246 = DIRECTION ( 'NONE',  ( 0.000000000000000000, 0.000000000000000000, -1.000000000000000000 ) ) ;
#13247 = CARTESIAN_POINT ( 'NONE',  ( 25.80383423833348644, -3.137017275366889901, -7.141595990038014818 ) ) ;
#13248 = ORIENTED_EDGE ( 'NONE', *, *, #8489, .T. ) ;
#13249 = CARTESIAN_POINT ( 'NONE',  ( 25.11802603177690330, -19.03270077640483038, 0.5379818257722508434 ) ) ;
#13250 = CARTESIAN_POINT ( 'NONE',  ( 33.10345976029034176, -2.594722134608779207, -3.283357778048662023 ) ) ;
#13251 = EDGE_CURVE ( 'NONE', #3432, #4167, #16521, .T. ) ;
#13252 = VECTOR ( 'NONE', #2031, 1000.000000000000227 ) ;
#13253 = ORIENTED_EDGE ( 'NONE', *, *, #6148, .T. ) ;
#13254 = CARTESIAN_POINT ( 'NONE',  ( 26.49461065740898036, -7.352653653197164019, -5.783357778048668685 ) ) ;
#13255 = CARTESIAN_POINT ( 'NONE',  ( 26.28374211850152875, -7.120308096563231715, -4.880631602441031447 ) ) ;
#13256 = LINE ( 'NONE', #838, #14102 ) ;
#13257 = DIRECTION ( 'NONE',  ( 0.9928203230275512992, 0.1196152422706610735, 9.614813431917828943E-17 ) ) ;
#13258 = CARTESIAN_POINT ( 'NONE',  ( 28.91555989733679866, -4.553094948490599592, -3.283357778048664688 ) ) ;
#13259 = CARTESIAN_POINT ( 'NONE',  ( 32.14213199643173624, -2.910415664685331638, -3.627061608673662896 ) ) ;
#13260 = EDGE_CURVE ( 'NONE', #9480, #7608, #10928, .T. ) ;
#13261 =( BOUNDED_CURVE ( )  B_SPLINE_CURVE ( 2, ( #10729, #6580, #12105, #8293, #14926, #5383, #15006, #17687, #5210 ),
 .UNSPECIFIED., .F., .T. ) 
 B_SPLINE_CURVE_WITH_KNOTS ( ( 3, 2, 2, 2, 3 ),
 ( 0.3269230769230769273, 0.3333333333333333148, 0.3461538461538461453, 0.3589743589743589758, 0.3653846153846154188 ),
 .UNSPECIFIED. ) 
 CURVE ( )  GEOMETRIC_REPRESENTATION_ITEM ( )  RATIONAL_B_SPLINE_CURVE ( ( 0.9330127018922194093, 0.9330127018922194093, 1.000000000000000000, 0.8660254037844387076, 1.000000000000000000, 0.8660254037844387076, 1.000000000000000000, 0.9330127018922190762, 0.9330127018922194093 ) ) 
 REPRESENTATION_ITEM ( '' )  );
#13262 = CIRCLE ( 'NONE', #11511, 5.000000000000000888 ) ;
#13263 = DIRECTION ( 'NONE',  ( 0.000000000000000000, -0.4999999999999992228, 0.8660254037844390407 ) ) ;
#13264 = PLANE ( 'NONE',  #16243 ) ;
#13265 = CIRCLE ( 'NONE', #17929, 2.000000000000001776 ) ;
#13266 = CARTESIAN_POINT ( 'NONE',  ( -0.3198814748697748067, -4.434118497892180599, -0.3507732604232522977 ) ) ;
#13267 = ORIENTED_EDGE ( 'NONE', *, *, #12361, .T. ) ;
#13268 = LINE ( 'NONE', #14644, #10776 ) ;
#13269 = CARTESIAN_POINT ( 'NONE',  ( 30.98067518586950442, -1.786210345264705790, -5.783357778048658027 ) ) ;
#13270 = CARTESIAN_POINT ( 'NONE',  ( 33.76207435632690590, -3.969185667289998332, -3.627061608673664672 ) ) ;
#13271 = FACE_OUTER_BOUND ( 'NONE', #10181, .T. ) ;
#13272 = CIRCLE ( 'NONE', #2834, 3.425051884552432035 ) ;
#13273 = EDGE_CURVE ( 'NONE', #12431, #15406, #17072, .T. ) ;
#13274 = CARTESIAN_POINT ( 'NONE',  ( 27.36943512155133362, -2.558652073080304845, -4.533357778048659803 ) ) ;
#13275 = DIRECTION ( 'NONE',  ( 0.9928203230275512992, 0.1196152422706610180, 4.006172263299093133E-17 ) ) ;
#13276 = CONTEXT_DEPENDENT_SHAPE_REPRESENTATION ( #10935, #6797 ) ;
#13277 = CARTESIAN_POINT ( 'NONE',  ( 0.000000000000000000, 0.000000000000000000, -2.000000000000000000 ) ) ;
#13278 = CARTESIAN_POINT ( 'NONE',  ( 0.000000000000000000, 0.000000000000000000, -4.000000000000000000 ) ) ;
#13279 = ORIENTED_EDGE ( 'NONE', *, *, #557, .T. ) ;
#13280 = CARTESIAN_POINT ( 'NONE',  ( 30.15443244188179150, -1.895953141405084086, -5.783357778048658027 ) ) ;
#13281 = FACE_OUTER_BOUND ( 'NONE', #11789, .T. ) ;
#13282 = CARTESIAN_POINT ( 'NONE',  ( 27.17934203385504333, -30.00000000000000355, 13.93658524716016878 ) ) ;
#13283 = EDGE_CURVE ( 'NONE', #13718, #6265, #16073, .T. ) ;
#13284 = CARTESIAN_POINT ( 'NONE',  ( 27.86926259684567597, -5.933094176093606897, 3.627061608673662896 ) ) ;
#13285 = ADVANCED_FACE ( 'NONE', ( #14429 ), #11522, .T. ) ;
#13286 = ORIENTED_EDGE ( 'NONE', *, *, #10691, .T. ) ;
#13287 =( BOUNDED_CURVE ( )  B_SPLINE_CURVE ( 2, ( #12082, #2326, #6739, #12177, #15082, #9364, #6829, #10543, #2665 ),
 .UNSPECIFIED., .F., .T. ) 
 B_SPLINE_CURVE_WITH_KNOTS ( ( 3, 2, 2, 2, 3 ),
 ( 0.2500000000000000000, 0.2564102564102563875, 0.2692307692307692180, 0.2820512820512820484, 0.2884615384615384914 ),
 .UNSPECIFIED. ) 
 CURVE ( )  GEOMETRIC_REPRESENTATION_ITEM ( )  RATIONAL_B_SPLINE_CURVE ( ( 0.9330127018922194093, 0.9330127018922195203, 1.000000000000000000, 0.8660254037844387076, 1.000000000000000000, 0.8660254037844387076, 1.000000000000000000, 0.9330127018922190762, 0.9330127018922194093 ) ) 
 REPRESENTATION_ITEM ( '' )  );
#13288 = ORIENTED_EDGE ( 'NONE', *, *, #5707, .F. ) ;
#13289 = CARTESIAN_POINT ( 'NONE',  ( 33.35047706458318828, -2.764833946905071560, 3.627061608673666893 ) ) ;
#13290 = CARTESIAN_POINT ( 'NONE',  ( 29.25000000000000000, -16.21813761408365195, -13.37255996287876236 ) ) ;
#13291 = CARTESIAN_POINT ( 'NONE',  ( 32.21340264088064487, -1.637691031382005669, -6.453230759126468818 ) ) ;
#13292 = ORIENTED_EDGE ( 'NONE', *, *, #2534, .F. ) ;
#13293 = CARTESIAN_POINT ( 'NONE',  ( 32.85952466860454280, -1.897204703373130741, -7.033357778048658027 ) ) ;
#13294 = AXIS2_PLACEMENT_3D ( 'NONE', #9574, #1346, #13767 ) ;
#13295 = DIRECTION ( 'NONE',  ( -0.000000000000000000, -0.000000000000000000, -1.000000000000000000 ) ) ;
#13296 = CYLINDRICAL_SURFACE ( 'NONE', #4125, 2.500000000000001776 ) ;
#13297 = FACE_OUTER_BOUND ( 'NONE', #10532, .T. ) ;
#13298 = VERTEX_POINT ( 'NONE', #14620 ) ;
#13299 = CARTESIAN_POINT ( 'NONE',  ( 31.28415083292585663, -5.521667582366822202, -3.627061608673667781 ) ) ;
#13300 = CARTESIAN_POINT ( 'NONE',  ( -2.725758460534118743, 3.045084772581732491, -2.920601398289153661 ) ) ;
#13301 = DIRECTION ( 'NONE',  ( 1.000000000000000000, 0.000000000000000000, 0.000000000000000000 ) ) ;
#13302 = CARTESIAN_POINT ( 'NONE',  ( 27.09860475545177039, -3.518061095420291995, -3.627061608673662896 ) ) ;
#13303 = AXIS2_PLACEMENT_3D ( 'NONE', #14191, #4927, #14472 ) ;
#13304 = PRODUCT ( 'o-rings series a_iso_O-ring 19x1.8-A-ISO 3601-1', 'o-rings series a_iso_O-ring 19x1.8-A-ISO 3601-1', '', ( #12833 ) ) ;
#13305 = CARTESIAN_POINT ( 'NONE',  ( 33.15485366002904755, -6.560422763297783177, -5.783357778048663356 ) ) ;
#13306 = DIRECTION ( 'NONE',  ( 0.9928203230275510771, 0.1196152422706609902, 4.006172263299092517E-17 ) ) ;
#13307 = CARTESIAN_POINT ( 'NONE',  ( 26.61898274975073164, -6.283600725846810953, -3.283357778048667797 ) ) ;
#13308 = CARTESIAN_POINT ( 'NONE',  ( 28.23639288985533824, -7.542548330185622874, 5.783357778048657138 ) ) ;
#13309 = CIRCLE ( 'NONE', #2322, 10.50000000000000000 ) ;
#13310 = VERTEX_POINT ( 'NONE', #7714 ) ;
#13311 = VERTEX_POINT ( 'NONE', #13239 ) ;
#13312 = ORIENTED_EDGE ( 'NONE', *, *, #16894, .T. ) ;
#13313 = ORIENTED_EDGE ( 'NONE', *, *, #4914, .F. ) ;
#13314 = EDGE_CURVE ( 'NONE', #9477, #5981, #4999, .T. ) ;
#13315 = CARTESIAN_POINT ( 'NONE',  ( 26.99805802979993885, -6.665027654307603022, 6.861505862736158257 ) ) ;
#13316 = AXIS2_PLACEMENT_3D ( 'NONE', #5298, #4137, #12107 ) ;
#13317 = CARTESIAN_POINT ( 'NONE',  ( 5.000000000000002665, 0.000000000000000000, -2.700000000000000622 ) ) ;
#13318 = ORIENTED_EDGE ( 'NONE', *, *, #1216, .F. ) ;
#13319 = CARTESIAN_POINT ( 'NONE',  ( 29.42969845347704450, -5.944964990802679594, -8.283357778048664244 ) ) ;
#13320 = CARTESIAN_POINT ( 'NONE',  ( 2.500000000000000000, -2.357898499370431722, 2.818925648462311528E-15 ) ) ;
#13321 = CARTESIAN_POINT ( 'NONE',  ( 27.75966235412334981, -2.811446176820259879, -4.705209693361160461 ) ) ;
#13322 = CARTESIAN_POINT ( 'NONE',  ( 29.38468146192651886, -6.677295441714964142, 4.533357778048659803 ) ) ;
#13323 = LINE ( 'NONE', #3632, #1197 ) ;
#13324 = VECTOR ( 'NONE', #5920, 1000.000000000000000 ) ;
#13325 = DIRECTION ( 'NONE',  ( 1.000000000000000000, 0.000000000000000000, 0.000000000000000000 ) ) ;
#13326 = CARTESIAN_POINT ( 'NONE',  ( 31.03132594549780876, -1.780107929003061473, -6.453230759126465266 ) ) ;
#13327 = EDGE_CURVE ( 'NONE', #4586, #2990, #4799, .T. ) ;
#13328 = CARTESIAN_POINT ( 'NONE',  ( 27.14244485254070938, -4.766720295129625029, -7.939653947423662039 ) ) ;
#13329 = CARTESIAN_POINT ( 'NONE',  ( 22.62608969754382215, -9.966271075498049470, 15.00374444583767897 ) ) ;
#13330 = CARTESIAN_POINT ( 'NONE',  ( 33.46007730730551799, -5.886481946178435010, -4.705209693361169343 ) ) ;
#13331 = CARTESIAN_POINT ( 'NONE',  ( 31.04338717100262102, -6.177645381738930297, -6.861505862736167138 ) ) ;
#13332 = ORIENTED_EDGE ( 'NONE', *, *, #9471, .F. ) ;
#13333 = CARTESIAN_POINT ( 'NONE',  ( 12.50000000000000000, 1.530808498934191521E-15, -8.722503561260788629 ) ) ;
#13334 = CARTESIAN_POINT ( 'NONE',  ( 33.76207435632690590, -3.969185667289998332, 7.939653947423662039 ) ) ;
#13335 = CIRCLE ( 'NONE', #5214, 2.499999999999998668 ) ;
#13336 = ORIENTED_EDGE ( 'NONE', *, *, #11408, .T. ) ;
#13337 = EDGE_CURVE ( 'NONE', #2327, #10575, #7168, .T. ) ;
#13338 = DIRECTION ( 'NONE',  ( -0.1196152422706621143, -0.9928203230275509661, 0.000000000000000000 ) ) ;
#13339 = CARTESIAN_POINT ( 'NONE',  ( 33.19286683830256379, -2.783822866615540459, -7.939653947423660263 ) ) ;
#13340 = VERTEX_POINT ( 'NONE', #9163 ) ;
#13341 = CARTESIAN_POINT ( 'NONE',  ( 28.21828588914510050, -7.155181690169023057, 5.113484796970857005 ) ) ;
#13342 = AXIS2_PLACEMENT_3D ( 'NONE', #13812, #1051, #12186 ) ;
#13343 = DIRECTION ( 'NONE',  ( 0.9237280213470682178, 0.3830490080632377170, 0.000000000000000000 ) ) ;
#13344 = CYLINDRICAL_SURFACE ( 'NONE', #8702, 2.500000000000001776 ) ;
#13345 = VECTOR ( 'NONE', #9960, 999.9999999999998863 ) ;
#13346 = CARTESIAN_POINT ( 'NONE',  ( 0.5276476219768818643, -4.314164656931400721, -3.020318136128620434 ) ) ;
#13347 = CARTESIAN_POINT ( 'NONE',  ( 31.30979230060565044, -7.172264396038955603, -5.783357778048669573 ) ) ;
#13348 = TOROIDAL_SURFACE ( 'NONE', #12768, 12.70000000000000284, 0.9000000000000003553 ) ;
#13349 = VERTEX_POINT ( 'NONE', #13333 ) ;
#13350 = ORIENTED_EDGE ( 'NONE', *, *, #11209, .F. ) ;
#13351 = CARTESIAN_POINT ( 'NONE',  ( 29.01637427789896151, -7.048830937829683840, -5.783357778048668685 ) ) ;
#13352 = CARTESIAN_POINT ( 'NONE',  ( -27.17934203385504333, -30.00000000000000355, -13.93658524716016878 ) ) ;
#13353 = CARTESIAN_POINT ( 'NONE',  ( 30.32207992551315812, -1.865558067907615802, -6.453230759126468818 ) ) ;
#13354 = CARTESIAN_POINT ( 'NONE',  ( 33.81344892038539740, -6.481075040654872943, -6.453230759126470595 ) ) ;
#13355 = CARTESIAN_POINT ( 'NONE',  ( 27.24942365487322959, -6.207645047004941574, -3.283357778048667797 ) ) ;
#13356 = CARTESIAN_POINT ( 'NONE',  ( 31.27962407439061110, -2.387360303286481855, -6.861505862736159145 ) ) ;
#13357 = CIRCLE ( 'NONE', #2084, 2.000000000000001776 ) ;
#13358 = ADVANCED_FACE ( 'NONE', ( #17549 ), #555, .T. ) ;
#13359 = CIRCLE ( 'NONE', #8431, 2.499999999999998668 ) ;
#13360 = ORIENTED_EDGE ( 'NONE', *, *, #9666, .T. ) ;
#13361 = LINE ( 'NONE', #3659, #8338 ) ;
#13362 = LINE ( 'NONE', #11991, #15950 ) ;
#13363 = ORIENTED_EDGE ( 'NONE', *, *, #83, .T. ) ;
#13364 = CARTESIAN_POINT ( 'NONE',  ( 10.47816170930907553, -0.6768509389586216951, -6.005572809000082835 ) ) ;
#13365 = CARTESIAN_POINT ( 'NONE',  ( 45.00000000000000711, -19.03270077640483038, 0.5379818257722508434 ) ) ;
#13366 = CARTESIAN_POINT ( 'NONE',  ( 0.000000000000000000, 0.000000000000000000, 0.000000000000000000 ) ) ;
#13367 = DIRECTION ( 'NONE',  ( 0.000000000000000000, 0.000000000000000000, -1.000000000000000000 ) ) ;
#13368 = PRESENTATION_LAYER_ASSIGNMENT (  '', '', ( #3231 ) ) ;
#13369 = CARTESIAN_POINT ( 'NONE',  ( 30.48043329534786849, -5.818372192732907067, -3.283357778048667797 ) ) ;
#13370 = CARTESIAN_POINT ( 'NONE',  ( -3.443595183066686438, -15.28297513750540837, -16.99984776326509106 ) ) ;
#13371 = CARTESIAN_POINT ( 'NONE',  ( 0.000000000000000000, 0.000000000000000000, -10.00000000000000000 ) ) ;
#13372 = DIRECTION ( 'NONE',  ( 1.000000000000000000, 0.000000000000000000, 0.000000000000000000 ) ) ;
#13373 = CARTESIAN_POINT ( 'NONE',  ( 29.03376756790819613, -4.538853258604016006, -7.939653947423662039 ) ) ;
#13374 = VECTOR ( 'NONE', #4882, 1000.000000000000000 ) ;
#13375 = CARTESIAN_POINT ( 'NONE',  ( 33.17094678975809074, -2.159493266760871499, -6.861505862736159145 ) ) ;
#13376 = CARTESIAN_POINT ( 'NONE',  ( 29.46348657678868577, -6.667800981652280967, 4.533357778048659803 ) ) ;
#13377 = CARTESIAN_POINT ( 'NONE',  ( 28.28502977505876359, -2.748149777785362957, 4.705209693361168455 ) ) ;
#13378 = EDGE_LOOP ( 'NONE', ( #12407, #15750, #154, #14769, #15839 ) ) ;
#13379 =( BOUNDED_CURVE ( )  B_SPLINE_CURVE ( 2, ( #10781, #10955, #1373, #105, #15158, #6718, #2905, #12259, #17827 ),
 .UNSPECIFIED., .F., .F. ) 
 B_SPLINE_CURVE_WITH_KNOTS ( ( 3, 2, 2, 2, 3 ),
 ( 0.3653846153846154188, 0.3717948717948718063, 0.3846153846153846367, 0.3974358974358974117, 0.4038461538461538547 ),
 .UNSPECIFIED. ) 
 CURVE ( )  GEOMETRIC_REPRESENTATION_ITEM ( )  RATIONAL_B_SPLINE_CURVE ( ( 0.9330127018922194093, 0.9330127018922196314, 1.000000000000000000, 0.8660254037844387076, 1.000000000000000000, 0.8660254037844387076, 1.000000000000000000, 0.9330127018922190762, 0.9330127018922194093 ) ) 
 REPRESENTATION_ITEM ( '' )  );
#13380 = VECTOR ( 'NONE', #16059, 1000.000000000000000 ) ;
#13381 = ORIENTED_EDGE ( 'NONE', *, *, #10085, .T. ) ;
#13382 = EDGE_CURVE ( 'NONE', #16631, #17480, #3715, .T. ) ;
#13383 = CARTESIAN_POINT ( 'NONE',  ( 31.56875459193803124, -6.114348982704044921, 6.861505862736157368 ) ) ;
#13384 = CARTESIAN_POINT ( 'NONE',  ( -28.06754645621478517, -12.55420304724502323, 13.70087619851170757 ) ) ;
#13385 = CARTESIAN_POINT ( 'NONE',  ( 4.281152949374537720, 4.203775615332211224, -1.901951201008075243 ) ) ;
#13386 = ORIENTED_EDGE ( 'NONE', *, *, #1420, .F. ) ;
#13387 = DIRECTION ( 'NONE',  ( 0.05980762113533047430, -0.4964101615137755941, -0.8660254037844387076 ) ) ;
#13388 = AXIS2_PLACEMENT_3D ( 'NONE', #13750, #1062, #5303 ) ;
#13389 = CIRCLE ( 'NONE', #9606, 6.249999999999998224 ) ;
#13390 = CARTESIAN_POINT ( 'NONE',  ( -2.000000000000005329, -3.464101615137750390, 0.000000000000000000 ) ) ;
#13391 = CARTESIAN_POINT ( 'NONE',  ( 34.43754810739937966, -7.916730809865823559, -5.783357778048663356 ) ) ;
#13392 = EDGE_CURVE ( 'NONE', #5056, #16729, #12400, .T. ) ;
#13393 = CARTESIAN_POINT ( 'NONE',  ( 31.66930131758986988, -2.967382423816733894, -3.627061608673662008 ) ) ;
#13394 = ADVANCED_FACE ( 'NONE', ( #7449 ), #15978, .T. ) ;
#13395 = CARTESIAN_POINT ( 'NONE',  ( 31.93198502805756789, -2.935734224299280548, -7.939653947423660263 ) ) ;
#13396 = CARTESIAN_POINT ( 'NONE',  ( 38.64694918415791136, -1.054552983374777986, -9.783357778048662468 ) ) ;
#13397 = CARTESIAN_POINT ( 'NONE',  ( 31.97277696464621854, -6.702839660918840536, -5.783357778048663356 ) ) ;
#13398 = CARTESIAN_POINT ( 'NONE',  ( 29.77044413525282707, -1.932019286686802895, -6.453230759126468818 ) ) ;
#13399 = AXIS2_PLACEMENT_3D ( 'NONE', #17485, #10790, #2404 ) ;
#13400 = LINE ( 'NONE', #16132, #536 ) ;
#13401 = CARTESIAN_POINT ( 'NONE',  ( 25.93714794488954212, -2.393855775999666591, -5.783357778048658027 ) ) ;
#13402 = AXIS2_PLACEMENT_3D ( 'NONE', #4131, #9637, #6760 ) ;
#13403 = CARTESIAN_POINT ( 'NONE',  ( 28.36392410707646761, -4.619556167269785796, 8.283357778048662468 ) ) ;
#13404 =( BOUNDED_CURVE ( )  B_SPLINE_CURVE ( 2, ( #6583, #5300, #2505, #3954, #8216, #1147, #6765, #12297, #10996 ),
 .UNSPECIFIED., .F., .T. ) 
 B_SPLINE_CURVE_WITH_KNOTS ( ( 3, 2, 2, 2, 3 ),
 ( 0.05769230769230771633, 0.06410256410256409687, 0.07692307692307692735, 0.08974358974358974395, 0.09615384615384617306 ),
 .UNSPECIFIED. ) 
 CURVE ( )  GEOMETRIC_REPRESENTATION_ITEM ( )  RATIONAL_B_SPLINE_CURVE ( ( 0.9330127018922194093, 0.9330127018922196314, 1.000000000000000000, 0.8660254037844387076, 1.000000000000000000, 0.8660254037844387076, 1.000000000000000000, 0.9330127018922191873, 0.9330127018922194093 ) ) 
 REPRESENTATION_ITEM ( '' )  );
#13405 = ORIENTED_EDGE ( 'NONE', *, *, #3743, .T. ) ;
#13406 = EDGE_LOOP ( 'NONE', ( #1160, #3029, #11673, #4300 ) ) ;
#13407 = ORIENTED_EDGE ( 'NONE', *, *, #15785, .F. ) ;
#13408 = ADVANCED_FACE ( 'NONE', ( #10241 ), #3546, .F. ) ;
#13409 = ORIENTED_EDGE ( 'NONE', *, *, #2917, .T. ) ;
#13410 = CARTESIAN_POINT ( 'NONE',  ( 30.12381574833269937, -2.526612381163247267, 6.861505862736165362 ) ) ;
#13411 = CARTESIAN_POINT ( 'NONE',  ( 30.82871344409320713, -3.068656662272551294, 3.627061608673666449 ) ) ;
#13412 = ORIENTED_EDGE ( 'NONE', *, *, #6791, .F. ) ;
#13413 = DIRECTION ( 'NONE',  ( -0.000000000000000000, -0.000000000000000000, 1.000000000000000000 ) ) ;
#13414 = CARTESIAN_POINT ( 'NONE',  ( 0.000000000000000000, 0.000000000000000000, 12.00000000000000000 ) ) ;
#13415 =( GEOMETRIC_REPRESENTATION_CONTEXT ( 3 ) GLOBAL_UNCERTAINTY_ASSIGNED_CONTEXT ( ( #5338 ) ) GLOBAL_UNIT_ASSIGNED_CONTEXT ( ( #12550, #2942, #15265 ) ) REPRESENTATION_CONTEXT ( 'NONE', 'WORKASPACE' ) );
#13416 = DIRECTION ( 'NONE',  ( -0.3830490080632376615, 0.9237280213470682178, 0.000000000000000000 ) ) ;
#13417 = CARTESIAN_POINT ( 'NONE',  ( 28.91999743871649997, -5.806501378023834370, -3.627061608673668225 ) ) ;
#13418 = CYLINDRICAL_SURFACE ( 'NONE', #13652, 13.00000000000000178 ) ;
#13419 = EDGE_CURVE ( 'NONE', #12118, #1069, #12685, .T. ) ;
#13420 = CIRCLE ( 'NONE', #3283, 3.999999999999994671 ) ;
#13421 = CARTESIAN_POINT ( 'NONE',  ( 31.71123609653335507, -2.762457591843783256, -8.283357778048658915 ) ) ;
#13422 = CARTESIAN_POINT ( 'NONE',  ( 3.000000000000000000, 0.000000000000000000, 13.31572692736085095 ) ) ;
#13423 = CARTESIAN_POINT ( 'NONE',  ( 27.65911562847151117, -5.958412735707574015, -3.627061608673668225 ) ) ;
#13424 = CARTESIAN_POINT ( 'NONE',  ( 16.91330062320331962, -14.78391025039656625, 16.01216328675237577 ) ) ;
#13425 =( LENGTH_UNIT ( ) NAMED_UNIT ( * ) SI_UNIT ( .MILLI., .METRE. ) );
#13426 = EDGE_CURVE ( 'NONE', #4804, #4963, #7803, .T. ) ;
#13427 = CARTESIAN_POINT ( 'NONE',  ( 32.69811611091622439, -2.216460025892273311, -6.861505862736158257 ) ) ;
#13428 = AXIS2_PLACEMENT_3D ( 'NONE', #15508, #14336, #16885 ) ;
#13429 = CARTESIAN_POINT ( 'NONE',  ( 33.43363050022580296, -2.127845067243429256, -4.705209693361160461 ) ) ;
#13430 = EDGE_LOOP ( 'NONE', ( #6262, #16228, #13682, #9495 ) ) ;
#13431 = CYLINDRICAL_SURFACE ( 'NONE', #1987, 2.499999999999999112 ) ;
#13432 = DIRECTION ( 'NONE',  ( 0.000000000000000000, 0.000000000000000000, -1.000000000000000000 ) ) ;
#13433 = VERTEX_POINT ( 'NONE', #10511 ) ;
#13434 = DIRECTION ( 'NONE',  ( 0.000000000000000000, 0.4999999999999991118, -0.8660254037844391517 ) ) ;
#13435 = CARTESIAN_POINT ( 'NONE',  ( 27.47505859511117521, -2.218764776483033163, -5.783357778048658915 ) ) ;
#13436 = DIRECTION ( 'NONE',  ( 0.000000000000000000, 0.000000000000000000, -1.000000000000000000 ) ) ;
#13437 = CARTESIAN_POINT ( 'NONE',  ( 28.64916707261694384, -6.765910400363817523, -4.533357778048668685 ) ) ;
#13438 = LINE ( 'NONE', #5251, #3782 ) ;
#13439 = CARTESIAN_POINT ( 'NONE',  ( 33.68284756902015431, -1.652629194728085338, -9.783357778048662468 ) ) ;
#13440 = CARTESIAN_POINT ( 'NONE',  ( 32.96459815279162342, -1.884545423566157174, -4.533357778048659803 ) ) ;
#13441 = ORIENTED_EDGE ( 'NONE', *, *, #938, .T. ) ;
#13442 = EDGE_CURVE ( 'NONE', #17902, #2263, #11693, .T. ) ;
#13443 = CARTESIAN_POINT ( 'NONE',  ( 32.34358231980129261, -4.140085944684206432, -3.627061608673664672 ) ) ;
#13444 = DIRECTION ( 'NONE',  ( 0.000000000000000000, -1.000000000000000000, 1.103561164596346103E-15 ) ) ;
#13445 = DIRECTION ( 'NONE',  ( 0.000000000000000000, 1.000000000000000000, 0.000000000000000000 ) ) ;
#13446 = CARTESIAN_POINT ( 'NONE',  ( 33.79776779778399032, -6.145605689821873163, -7.033357778048666908 ) ) ;
#13447 = DIRECTION ( 'NONE',  ( 0.000000000000000000, -0.000000000000000000, 1.000000000000000000 ) ) ;
#13448 = CARTESIAN_POINT ( 'NONE',  ( 30.65370992780335868, -5.597623261208692469, -3.627061608673667781 ) ) ;
#13449 = VECTOR ( 'NONE', #8351, 1000.000000000000227 ) ;
#13450 = EDGE_CURVE ( 'NONE', #7608, #9808, #10360, .T. ) ;
#13451 = EDGE_CURVE ( 'NONE', #7372, #9007, #14789, .T. ) ;
#13452 = ORIENTED_EDGE ( 'NONE', *, *, #8873, .F. ) ;
#13453 = VERTEX_POINT ( 'NONE', #13775 ) ;
#13454 = CARTESIAN_POINT ( 'NONE',  ( 9.458171371211012257, -3.728626979641465500, -2.666481567098319072 ) ) ;
#13455 = CARTESIAN_POINT ( 'NONE',  ( -28.84390385427241199, -13.99246034770667713, -13.48718205731130304 ) ) ;
#13456 = EDGE_LOOP ( 'NONE', ( #8771, #4547, #3963, #11354 ) ) ;
#13457 = DIRECTION ( 'NONE',  ( -0.9928203230275512992, -0.1196152422706610180, -4.006172263299093133E-17 ) ) ;
#13458 = PRODUCT_DEFINITION_SHAPE ( 'NONE', 'NONE',  #17971 ) ;
#13460 = EDGE_LOOP ( 'NONE', ( #15219, #16365, #13222, #2342 ) ) ;
#13459 = CARTESIAN_POINT ( 'NONE',  ( 15.92260893619738837, -28.39189527176317540, 16.15082599432113142 ) ) ;
#13461 = CARTESIAN_POINT ( 'NONE',  ( 32.69811611091622439, -2.216460025892273311, -6.861505862736158257 ) ) ;
#13462 = EDGE_LOOP ( 'NONE', ( #10837, #8899, #8244, #5379 ) ) ;
#13463 = CARTESIAN_POINT ( 'NONE',  ( -34.91600907648203389, -11.88801210197604341, 0.000000000000000000 ) ) ;
#13464 = ADVANCED_FACE ( 'NONE', ( #8156 ), #13431, .F. ) ;
#13465 = CARTESIAN_POINT ( 'NONE',  ( 33.30246708102489350, -5.905470865888903020, -4.705209693361168455 ) ) ;
#13466 = DIRECTION ( 'NONE',  ( 0.000000000000000000, 0.000000000000000000, 1.000000000000000000 ) ) ;
#13467 = EDGE_CURVE ( 'NONE', #6659, #9791, #15834, .T. ) ;
#13468 = DIRECTION ( 'NONE',  ( 0.000000000000000000, -1.000000000000000000, 0.000000000000000000 ) ) ;
#13469 = DIRECTION ( 'NONE',  ( -1.000000000000000000, -0.000000000000000000, -0.000000000000000000 ) ) ;
#13470 = VERTEX_POINT ( 'NONE', #6874 ) ;
#13471 = CARTESIAN_POINT ( 'NONE',  ( 30.93831368681553684, -6.190304661545915188, -4.705209693361169343 ) ) ;
#13472 = CARTESIAN_POINT ( 'NONE',  ( 2.500000000000000888, 3.061616997868384127E-16, -4.674599999999997202 ) ) ;
#13473 = CARTESIAN_POINT ( 'NONE',  ( 33.06225340847440464, -6.234220648470727433, 7.033357778048657138 ) ) ;
#13474 = ORIENTED_EDGE ( 'NONE', *, *, #3875, .F. ) ;
#13475 = CARTESIAN_POINT ( 'NONE',  ( 29.04699097144805364, -6.418171698071525100, 6.861505862736157368 ) ) ;
#13476 = CARTESIAN_POINT ( 'NONE',  ( 28.48022645605872327, -3.151730446115816875, 3.283357778048666464 ) ) ;
#13477 = ORIENTED_EDGE ( 'NONE', *, *, #2848, .F. ) ;
#13478 = LINE ( 'NONE', #9298, #9060 ) ;
#13479 = DIRECTION ( 'NONE',  ( 0.000000000000000000, 1.000000000000000000, 0.000000000000000000 ) ) ;
#13480 = ORIENTED_EDGE ( 'NONE', *, *, #1252, .T. ) ;
#13481 = CARTESIAN_POINT ( 'NONE',  ( 26.31065902414478330, -7.328232685206446106, -6.312034385895062272 ) ) ;
#13482 = CARTESIAN_POINT ( 'NONE',  ( 31.43723430067123914, -2.368371383576012956, -6.861505862736158257 ) ) ;
#13483 = CARTESIAN_POINT ( 'NONE',  ( 0.02448804030507906182, 4.877043185438126649, -3.451162025751988160 ) ) ;
#13484 = FACE_OUTER_BOUND ( 'NONE', #1577, .T. ) ;
#13485 =( LENGTH_UNIT ( ) NAMED_UNIT ( * ) SI_UNIT ( .MILLI., .METRE. ) );
#13486 = CARTESIAN_POINT ( 'NONE',  ( 25.72395281601508898, -4.937620572523835349, 3.627061608673664228 ) ) ;
#13487 =( BOUNDED_CURVE ( )  B_SPLINE_CURVE ( 2, ( #12151, #6985, #15689, #3089, #7441, #4616, #2899, #5694, #8429 ),
 .UNSPECIFIED., .F., .T. ) 
 B_SPLINE_CURVE_WITH_KNOTS ( ( 3, 2, 2, 2, 3 ),
 ( 0.6730769230769231282, 0.6794871794871795156, 0.6923076923076922906, 0.7051282051282051766, 0.7115384615384615641 ),
 .UNSPECIFIED. ) 
 CURVE ( )  GEOMETRIC_REPRESENTATION_ITEM ( )  RATIONAL_B_SPLINE_CURVE ( ( 0.9330127018922192983, 0.9330127018922198534, 1.000000000000000000, 0.8660254037844387076, 1.000000000000000000, 0.8660254037844387076, 1.000000000000000000, 0.9330127018922194093, 0.9330127018922194093 ) ) 
 REPRESENTATION_ITEM ( '' )  );
#13488 = EDGE_CURVE ( 'NONE', #9311, #5626, #6795, .T. ) ;
#13489 = CARTESIAN_POINT ( 'NONE',  ( 33.04340326765378677, -1.875050963503474222, 7.033357778048666020 ) ) ;
#13490 = CARTESIAN_POINT ( 'NONE',  ( 28.19013153391124860, -7.158573733970061248, -5.783357778048657138 ) ) ;
#13491 = DIRECTION ( 'NONE',  ( -1.000000000000000000, 0.000000000000000000, 0.000000000000000000 ) ) ;
#13492 = CARTESIAN_POINT ( 'NONE',  ( 29.35841309260160159, -6.680460261459264970, 7.033357778048657138 ) ) ;
#13493 = ORIENTED_EDGE ( 'NONE', *, *, #12160, .T. ) ;
#13494 = ADVANCED_FACE ( 'NONE', ( #9332 ), #12097, .F. ) ;
#13495 = ORIENTED_EDGE ( 'NONE', *, *, #218, .T. ) ;
#13496 = ORIENTED_EDGE ( 'NONE', *, *, #7404, .F. ) ;
#13497 = CARTESIAN_POINT ( 'NONE',  ( 31.25770402584614516, -1.763030703431812674, 5.783357778048668685 ) ) ;
#13498 = CARTESIAN_POINT ( 'NONE',  ( 30.80679339554874119, -2.444327062417882779, 4.705209693361168455 ) ) ;
#13499 = VERTEX_POINT ( 'NONE', #2535 ) ;
#13500 = CYLINDRICAL_SURFACE ( 'NONE', #16198, 2.500000000000000000 ) ;
#13501 = CARTESIAN_POINT ( 'NONE',  ( 30.10960860451258370, -6.927314653643411368, -6.453230759126470595 ) ) ;
#13502 = CARTESIAN_POINT ( 'NONE',  ( -35.74085044863416272, -23.57886868891566223, -11.27079897466147607 ) ) ;
#13503 = CARTESIAN_POINT ( 'NONE',  ( 30.41294626588012306, -6.253601060580800564, -6.861505862736167138 ) ) ;
#13504 = DIRECTION ( 'NONE',  ( -0.1196152422706614343, 0.9928203230275510771, 0.000000000000000000 ) ) ;
#13505 = CARTESIAN_POINT ( 'NONE',  ( 28.53771668024168662, -2.080538600569502794, -5.783357778048658027 ) ) ;
#13506 = PLANE ( 'NONE',  #13965 ) ;
#13507 = DIRECTION ( 'NONE',  ( 0.000000000000000000, 0.000000000000000000, -1.000000000000000000 ) ) ;
#13508 = CARTESIAN_POINT ( 'NONE',  ( -17.24286622940504188, 11.12094428624988218, 15.96573730347181019 ) ) ;
#13509 =( LENGTH_UNIT ( ) NAMED_UNIT ( * ) SI_UNIT ( .MILLI., .METRE. ) );
#13510 = ORIENTED_EDGE ( 'NONE', *, *, #3300, .T. ) ;
#13511 = EDGE_CURVE ( 'NONE', #2866, #17749, #15832, .T. ) ;
#13512 =( BOUNDED_CURVE ( )  B_SPLINE_CURVE ( 2, ( #6384, #13188, #5098, #14648, #766, #14817, #6292, #11813, #17391 ),
 .UNSPECIFIED., .F., .T. ) 
 B_SPLINE_CURVE_WITH_KNOTS ( ( 3, 2, 2, 2, 3 ),
 ( 0.4038461538461538547, 0.4102564102564102422, 0.4230769230769230727, 0.4358974358974359031, 0.4423076923076923461 ),
 .UNSPECIFIED. ) 
 CURVE ( )  GEOMETRIC_REPRESENTATION_ITEM ( )  RATIONAL_B_SPLINE_CURVE ( ( 0.9330127018922194093, 0.9330127018922196314, 1.000000000000000000, 0.8660254037844387076, 1.000000000000000000, 0.8660254037844387076, 1.000000000000000000, 0.9330127018922190762, 0.9330127018922194093 ) ) 
 REPRESENTATION_ITEM ( '' )  );
#13513 = CARTESIAN_POINT ( 'NONE',  ( 32.28234893270314387, -5.401404424200516807, -7.939653947423664704 ) ) ;
#13514 = CARTESIAN_POINT ( 'NONE',  ( 33.46007730730551799, -5.886481946178435010, -4.705209693361169343 ) ) ;
#13515 = ORIENTED_EDGE ( 'NONE', *, *, #4448, .F. ) ;
#13516 = CARTESIAN_POINT ( 'NONE',  ( 15.92260893619738837, -28.39189527176317540, 6.000000000000000000 ) ) ;
#13517 = CARTESIAN_POINT ( 'NONE',  ( 26.18945719470476163, -6.341381504099093291, 3.746363773741651304 ) ) ;
#13518 = EDGE_CURVE ( 'NONE', #4359, #2334, #16744, .T. ) ;
#13519 = ORIENTED_EDGE ( 'NONE', *, *, #7285, .T. ) ;
#13520 = CARTESIAN_POINT ( 'NONE',  ( 33.27602027394517847, -2.146833986953896822, 6.861505862736165362 ) ) ;
#13521 = CARTESIAN_POINT ( 'NONE',  ( 28.56093688906631911, -4.595820017735426255, -3.627061608673664672 ) ) ;
#13522 = CARTESIAN_POINT ( 'NONE',  ( 8.632250723006720250, -18.84644399697197770, -13.00000000000000178 ) ) ;
#13523 = CARTESIAN_POINT ( 'NONE',  ( 13.00000000000000178, 0.000000000000000000, 12.00000000000000000 ) ) ;
#13524 = CARTESIAN_POINT ( 'NONE',  ( 26.01652455409633902, -4.902371455920926380, 5.783357778048663356 ) ) ;
#13525 = DIRECTION ( 'NONE',  ( -0.000000000000000000, -0.000000000000000000, 1.000000000000000000 ) ) ;
#13526 = CARTESIAN_POINT ( 'NONE',  ( 30.30397292480292037, -1.478191427891014431, -5.783357778048658027 ) ) ;
#13527 = AXIS2_PLACEMENT_3D ( 'NONE', #6717, #10527, #16174 ) ;
#13528 = ORIENTED_EDGE ( 'NONE', *, *, #13897, .F. ) ;
#13529 = CARTESIAN_POINT ( 'NONE',  ( 32.51858583609114106, -1.611119345748072362, -5.783357778048658027 ) ) ;
#13530 = LINE ( 'NONE', #2303, #9309 ) ;
#13531 = CARTESIAN_POINT ( 'NONE',  ( 23.00000000000000000, -16.21813761408365195, -13.00000000000000178 ) ) ;
#13532 = CARTESIAN_POINT ( 'NONE',  ( 9.700633612364448766, 16.10095840566074799, -16.79370834700961979 ) ) ;
#13533 = FACE_OUTER_BOUND ( 'NONE', #2439, .T. ) ;
#13534 = CIRCLE ( 'NONE', #12362, 6.249999999999998224 ) ;
#13535 = CARTESIAN_POINT ( 'NONE',  ( 31.30154412293507349, -3.011689903141150815, -7.939653947423660263 ) ) ;
#13536 = ORIENTED_EDGE ( 'NONE', *, *, #7038, .T. ) ;
#13537 = VERTEX_POINT ( 'NONE', #9243 ) ;
#13538 = DIRECTION ( 'NONE',  ( 0.000000000000000000, 0.000000000000000000, 1.000000000000000000 ) ) ;
#13539 = EDGE_CURVE ( 'NONE', #17950, #6794, #14998, .T. ) ;
#13540 = CARTESIAN_POINT ( 'NONE',  ( -0.6666666666666676289, -4.233901974057269868, -3.000726591567087098 ) ) ;
#13541 = ORIENTED_EDGE ( 'NONE', *, *, #2690, .T. ) ;
#13542 = FILL_AREA_STYLE_COLOUR ( '', #5007 ) ;
#13543 = VECTOR ( 'NONE', #8794, 1000.000000000000227 ) ;
#13544 = CARTESIAN_POINT ( 'NONE',  ( 32.72003615946069743, -2.840789625746940938, -7.939653947423660263 ) ) ;
#13545 = CARTESIAN_POINT ( 'NONE',  ( 7.499998387031003411, -20.49508120620799900, 12.00000000000000000 ) ) ;
#13546 = ADVANCED_FACE ( 'NONE', ( #10931 ), #1714, .T. ) ;
#13547 = CARTESIAN_POINT ( 'NONE',  ( 33.28924367748503244, -4.026152426421394814, -7.939653947423662039 ) ) ;
#13548 = CARTESIAN_POINT ( 'NONE',  ( 4.024499207728656103, -2.323545700935583547, -3.272172305156509697 ) ) ;
#13549 = DIRECTION ( 'NONE',  ( 0.000000000000000000, 0.000000000000000000, 1.000000000000000000 ) ) ;
#13550 = CARTESIAN_POINT ( 'NONE',  ( 33.52375369703867847, -2.544085015380856518, -8.283357778048658915 ) ) ;
#13551 = DIRECTION ( 'NONE',  ( -1.000000000000000000, -1.501955125927555231E-12, 0.000000000000000000 ) ) ;
#13552 = CARTESIAN_POINT ( 'NONE',  ( 31.66250999073069750, -5.675955295111851484, 8.283357778048658915 ) ) ;
#13553 = EDGE_CURVE ( 'NONE', #11836, #17698, #432, .T. ) ;
#13554 = CARTESIAN_POINT ( 'NONE',  ( 28.49970350196817392, -5.857138497251738407, 3.627061608673662896 ) ) ;
#13555 =( LENGTH_UNIT ( ) NAMED_UNIT ( * ) SI_UNIT ( .MILLI., .METRE. ) );
#13556 = CARTESIAN_POINT ( 'NONE',  ( 28.60033944477555323, -4.591072787911525843, 3.283357778048664244 ) ) ;
#13557 = EDGE_CURVE ( 'NONE', #7755, #1473, #16497, .T. ) ;
#13558 = EDGE_LOOP ( 'NONE', ( #13292, #10124, #16633, #4050 ) ) ;
#13559 = VECTOR ( 'NONE', #13794, 1000.000000000000000 ) ;
#13560 = EDGE_LOOP ( 'NONE', ( #11595, #17697, #4919, #7019, #7627, #13845 ) ) ;
#13561 = LINE ( 'NONE', #5557, #9534 ) ;
#13562 = DIRECTION ( 'NONE',  ( -0.1196152422706620172, 0.9928203230275510771, 0.000000000000000000 ) ) ;
#13563 = CARTESIAN_POINT ( 'NONE',  ( 30.93831368681553684, -6.190304661545915188, -4.705209693361169343 ) ) ;
#13564 = CIRCLE ( 'NONE', #6906, 2.705189185291143605 ) ;
#13565 = DIRECTION ( 'NONE',  ( -1.000000000000000000, 0.000000000000000000, 0.000000000000000000 ) ) ;
#13566 = AXIS2_PLACEMENT_3D ( 'NONE', #5216, #5046, #5128 ) ;
#13567 = CARTESIAN_POINT ( 'NONE',  ( 30.03080348965042745, -6.936809113706096319, 5.113484796970857005 ) ) ;
#13568 = DIRECTION ( 'NONE',  ( 0.000000000000000000, 0.000000000000000000, -1.000000000000000000 ) ) ;
#13569 = CARTESIAN_POINT ( 'NONE',  ( 26.49461065740898036, -7.352653653197164019, 5.783357778048658027 ) ) ;
#13570 = CARTESIAN_POINT ( 'NONE',  ( 30.12381574833269937, -2.526612381163247267, 6.861505862736165362 ) ) ;
#13571 = FACE_OUTER_BOUND ( 'NONE', #2571, .T. ) ;
#13572 = CYLINDRICAL_SURFACE ( 'NONE', #12690, 2.500000000000001776 ) ;
#13573 = CARTESIAN_POINT ( 'NONE',  ( 32.06767520579373354, -2.292415704734142690, 4.705209693361168455 ) ) ;
#13574 = CARTESIAN_POINT ( 'NONE',  ( 27.36943512155133362, -2.558652073080304845, 7.033357778048666020 ) ) ;
#13575 = ORIENTED_EDGE ( 'NONE', *, *, #3292, .T. ) ;
#13576 = ORIENTED_EDGE ( 'NONE', *, *, #6749, .T. ) ;
#13577 = VECTOR ( 'NONE', #5200, 1000.000000000000227 ) ;
#13578 = VERTEX_POINT ( 'NONE', #1088 ) ;
#13579 = EDGE_CURVE ( 'NONE', #3428, #4413, #10939, .T. ) ;
#13580 = CARTESIAN_POINT ( 'NONE',  ( 30.86385689617752348, -5.572304701594726239, 3.627061608673662896 ) ) ;
#13581 = CARTESIAN_POINT ( 'NONE',  ( 28.50956232500783472, -2.083930644370540985, -6.453230759126464378 ) ) ;
#13582 = CARTESIAN_POINT ( 'NONE',  ( 29.80442540930208750, -6.953886339277345563, 5.783357778048657138 ) ) ;
#13583 = ORIENTED_EDGE ( 'NONE', *, *, #1381, .T. ) ;
#13584 = CARTESIAN_POINT ( 'NONE',  ( 30.03006034954003667, -2.965006068755446478, 8.283357778048666020 ) ) ;
#13585 = ADVANCED_FACE ( 'NONE', ( #12140 ), #17721, .F. ) ;
#13586 = CARTESIAN_POINT ( 'NONE',  ( 26.31556265977298992, -7.384422263489805793, -5.783357778048663356 ) ) ;
#13587 = CARTESIAN_POINT ( 'NONE',  ( 30.08145424927873535, -6.930706697444451336, -5.783357778048663356 ) ) ;
#13588 = CARTESIAN_POINT ( 'NONE',  ( 31.02146712245815507, -5.553315781884258229, -7.939653947423664704 ) ) ;
#13589 = CARTESIAN_POINT ( 'NONE',  ( 31.61111609099199171, -1.710254666422835745, -5.783357778048661579 ) ) ;
#13590 = AXIS2_PLACEMENT_3D ( 'NONE', #5190, #5102, #14738 ) ;
#13591 = CARTESIAN_POINT ( 'NONE',  ( 31.92138306490751987, -2.737139032229836122, -3.283357778048662023 ) ) ;
#13592 = CARTESIAN_POINT ( 'NONE',  ( 2.500000000000000000, 1.178949249685213863, -2.042000000000001148 ) ) ;
#13593 = CARTESIAN_POINT ( 'NONE',  ( 17.08564552898659272, -14.18688536295006664, -15.98696333172761719 ) ) ;
#13594 = CARTESIAN_POINT ( 'NONE',  ( 32.87199790123699472, -1.558343308739095656, -5.783357778048663356 ) ) ;
#13595 = EDGE_CURVE ( 'NONE', #8375, #5422, #3901, .T. ) ;
#13596 = CARTESIAN_POINT ( 'NONE',  ( 32.32618902979206865, -6.650063623909865385, -5.783357778048669573 ) ) ;
#13597 = CARTESIAN_POINT ( 'NONE',  ( 30.39102621733566423, -5.629271460726127607, -7.939653947423662927 ) ) ;
#13598 = EDGE_LOOP ( 'NONE', ( #2147, #7411 ) ) ;
#13599 = CARTESIAN_POINT ( 'NONE',  ( 33.76207435632690590, -3.969185667289998332, -3.627061608673664672 ) ) ;
#13600 = LINE ( 'NONE', #6261, #4943 ) ;
#13601 = VECTOR ( 'NONE', #4773, 1000.000000000000000 ) ;
#13602 = PRODUCT_DEFINITION_SHAPE ( 'NONE', 'NONE',  #17969 ) ;
#13603 = EDGE_LOOP ( 'NONE', ( #5301, #12026 ) ) ;
#13604 = ORIENTED_EDGE ( 'NONE', *, *, #532, .T. ) ;
#13605 = CARTESIAN_POINT ( 'NONE',  ( 32.12473870642251939, -5.420393343910986594, 3.627061608673662896 ) ) ;
#13606 = CARTESIAN_POINT ( 'NONE',  ( 26.86653773853314320, -2.919050055179571945, -6.861505862736159145 ) ) ;
#13607 = CIRCLE ( 'NONE', #10960, 2.000000000000001776 ) ;
#13608 = EDGE_CURVE ( 'NONE', #11785, #6928, #7492, .T. ) ;
#13609 = CARTESIAN_POINT ( 'NONE',  ( 0.000000000000000000, 0.000000000000000000, -10.50000000000000000 ) ) ;
#13610 = FACE_OUTER_BOUND ( 'NONE', #5201, .T. ) ;
#13611 = CARTESIAN_POINT ( 'NONE',  ( 25.78162057792671291, -2.952641328940848631, 6.684592198966492482 ) ) ;
#13612 = DIRECTION ( 'NONE',  ( 5.026720092345836698E-22, -4.581671729415424240E-22, 1.000000000000000000 ) ) ;
#13613 = CARTESIAN_POINT ( 'NONE',  ( 32.85952466860454280, -1.897204703373130741, -7.033357778048658027 ) ) ;
#13614 = ADVANCED_FACE ( 'NONE', ( #169, #6970 ), #12499, .T. ) ;
#13615 = VERTEX_POINT ( 'NONE', #4431 ) ;
#13616 = CARTESIAN_POINT ( 'NONE',  ( 32.01513846370018967, -2.298745344637636912, -4.705209693361161349 ) ) ;
#13617 = DIRECTION ( 'NONE',  ( -1.000000000000000000, 0.000000000000000000, 0.000000000000000000 ) ) ;
#13618 = CARTESIAN_POINT ( 'NONE',  ( 5.500000000000000888, -20.49999999999999645, 12.00000000000000000 ) ) ;
#13619 = DIRECTION ( 'NONE',  ( 0.000000000000000000, 0.000000000000000000, -1.000000000000000000 ) ) ;
#13620 = APPLICATION_CONTEXT ( 'automotive_design' ) ;
#13621 = CARTESIAN_POINT ( 'NONE',  ( -2.756166666307358071, -3.027528586792987753, -2.923144239647250231 ) ) ;
#13622 = AXIS2_PLACEMENT_3D ( 'NONE', #17683, #3865, #12193 ) ;
#13623 = CARTESIAN_POINT ( 'NONE',  ( 28.99445422935450267, -6.424501337975009996, -6.861505862736166250 ) ) ;
#13624 = AXIS2_PLACEMENT_3D ( 'NONE', #14820, #6561, #2410 ) ;
#13625 = DIRECTION ( 'NONE',  ( 0.9899494936611662466, 0.1414213562373111965, 0.000000000000000000 ) ) ;
#13626 = EDGE_CURVE ( 'NONE', #8959, #13130, #8654, .T. ) ;
#13627 = CARTESIAN_POINT ( 'NONE',  ( -26.79938379600875109, -11.23877132507977805, -14.03531701109484331 ) ) ;
#13628 = EDGE_LOOP ( 'NONE', ( #5648, #13065, #4029, #14625 ) ) ;
#13629 = CARTESIAN_POINT ( 'NONE',  ( 26.14833026707293229, -5.996374093462649491, 3.562504011865185838 ) ) ;
#13630 = ORIENTED_EDGE ( 'NONE', *, *, #16836, .T. ) ;
#13631 = CARTESIAN_POINT ( 'NONE',  ( 28.93739072872572393, -3.296523698798161650, -7.939653947423660263 ) ) ;
#13632 = FACE_OUTER_BOUND ( 'NONE', #15046, .T. ) ;
#13633 = CARTESIAN_POINT ( 'NONE',  ( 32.77709966008947617, -5.968767264923789284, -6.861505862736166250 ) ) ;
#13634 = LINE ( 'NONE', #1580, #219 ) ;
#13635 = VECTOR ( 'NONE', #12141, 1000.000000000000000 ) ;
#13636 = CARTESIAN_POINT ( 'NONE',  ( 27.89118264539014547, -6.557423775948280742, -6.861505862736167138 ) ) ;
#13637 = ADVANCED_FACE ( 'NONE', ( #8509 ), #9670, .T. ) ;
#13638 = CARTESIAN_POINT ( 'NONE',  ( 28.59863824134335530, -19.00380184606325429, -13.55546330914018149 ) ) ;
#13639 = VECTOR ( 'NONE', #16781, 1000.000000000000227 ) ;
#13640 = CARTESIAN_POINT ( 'NONE',  ( 29.97942892559193950, -4.424919740341219487, 7.939653947423662039 ) ) ;
#13641 = CARTESIAN_POINT ( 'NONE',  ( 30.71189515440122975, -6.854751018602581958, 5.783357778048664244 ) ) ;
#13642 = CARTESIAN_POINT ( 'NONE',  ( 23.84191717697471091, -22.42419738538529472, 14.74207411150917757 ) ) ;
#13643 = AXIS2_PLACEMENT_3D ( 'NONE', #12874, #6055, #4701 ) ;
#13644 = EDGE_LOOP ( 'NONE', ( #12620, #8987, #13162, #2606 ) ) ;
#13645 = AXIS2_PLACEMENT_3D ( 'NONE', #16263, #11889, #7909 ) ;
#13646 = CARTESIAN_POINT ( 'NONE',  ( 34.23532670761333918, -6.238269840783189579, -1.783357778048662690 ) ) ;
#13647 = EDGE_LOOP ( 'NONE', ( #1212, #2753 ) ) ;
#13648 = CARTESIAN_POINT ( 'NONE',  ( -20.00000000000000000, -30.00000000000000355, 17.00000000000000000 ) ) ;
#13649 = ORIENTED_EDGE ( 'NONE', *, *, #16607, .T. ) ;
#13650 = CARTESIAN_POINT ( 'NONE',  ( 26.56758885001203652, -2.317900097157796324, -5.783357778048670461 ) ) ;
#13651 = CARTESIAN_POINT ( 'NONE',  ( 30.43486631442457835, -6.877930660435475296, -5.783357778048669573 ) ) ;
#13652 = AXIS2_PLACEMENT_3D ( 'NONE', #10661, #14861, #16233 ) ;
#13653 = CARTESIAN_POINT ( 'NONE',  ( -2.016448651773435938E-27, -20.49999999999999645, 12.00000000000000000 ) ) ;
#13654 = DIRECTION ( 'NONE',  ( -0.5999999999999999778, 0.7999999999999999334, 0.000000000000000000 ) ) ;
#13655 =( NAMED_UNIT ( * ) SI_UNIT ( $, .STERADIAN. ) SOLID_ANGLE_UNIT ( ) );
#13656 = CARTESIAN_POINT ( 'NONE',  ( -5.499998817156067865, -20.49639288455253450, -6.000000000000000000 ) ) ;
#13657 = CARTESIAN_POINT ( 'NONE',  ( 28.10549950023366961, -2.142809097641162897, 5.783357778048668685 ) ) ;
#13658 = EDGE_CURVE ( 'NONE', #2496, #6942, #7838, .T. ) ;
#13659 = DIRECTION ( 'NONE',  ( 0.000000000000000000, -0.8660254037844390407, -0.4999999999999992784 ) ) ;
#13660 = DIRECTION ( 'NONE',  ( -0.000000000000000000, -0.000000000000000000, -1.000000000000000000 ) ) ;
#13661 = VECTOR ( 'NONE', #3888, 1000.000000000000000 ) ;
#13662 = CARTESIAN_POINT ( 'NONE',  ( 32.95662993491455950, -6.574107945067995118, 5.783357778048657138 ) ) ;
#13663 = ORIENTED_EDGE ( 'NONE', *, *, #2959, .T. ) ;
#13664 = ORIENTED_EDGE ( 'NONE', *, *, #3245, .T. ) ;
#13665 = VECTOR ( 'NONE', #4527, 1000.000000000000000 ) ;
#13666 = ORIENTED_EDGE ( 'NONE', *, *, #10315, .T. ) ;
#13667 = CARTESIAN_POINT ( 'NONE',  ( 32.64557936882268052, -2.222789665795767089, 6.861505862736165362 ) ) ;
#13668 = DIRECTION ( 'NONE',  ( 0.7752790601682274518, -0.5233950504778107637, 0.3535533905932737864 ) ) ;
#13669 = ORIENTED_EDGE ( 'NONE', *, *, #2109, .T. ) ;
#13670 = CARTESIAN_POINT ( 'NONE',  ( 29.17398450417959310, -7.029842018119214941, 5.783357778048657138 ) ) ;
#13671 = ORIENTED_EDGE ( 'NONE', *, *, #5131, .T. ) ;
#13672 = DIRECTION ( 'NONE',  ( 0.000000000000000000, 0.000000000000000000, 1.000000000000000000 ) ) ;
#13673 = CARTESIAN_POINT ( 'NONE',  ( 35.62429925076629189, -17.76690233603958902, 0.5379818257722508434 ) ) ;
#13674 = DIRECTION ( 'NONE',  ( -0.000000000000000000, 0.000000000000000000, -1.000000000000000000 ) ) ;
#13676 = AXIS2_PLACEMENT_3D ( 'NONE', #2868, #12479, #1258 ) ;
#13675 = CARTESIAN_POINT ( 'NONE',  ( 26.39823381822651882, -6.110324093391315436, -3.627061608673668225 ) ) ;
#13677 = CARTESIAN_POINT ( 'NONE',  ( 28.82057243903374655, -7.082618055128190093, -5.783357778048668685 ) ) ;
#13678 = CARTESIAN_POINT ( 'NONE',  ( 27.89480254248674740, -2.495355674045408367, -7.033357778048658027 ) ) ;
#13679 = CARTESIAN_POINT ( 'NONE',  ( 31.67744797322171735, -2.039621600994187656, 4.533357778048667797 ) ) ;
#13680 = CARTESIAN_POINT ( 'NONE',  ( 17.39700462756752231, -13.41815250082780508, -15.94071721526680108 ) ) ;
#13681 = DIRECTION ( 'NONE',  ( 1.000000000000000000, 0.000000000000000000, 0.000000000000000000 ) ) ;
#13682 = ORIENTED_EDGE ( 'NONE', *, *, #8965, .F. ) ;
#13683 = AXIS2_PLACEMENT_3D ( 'NONE', #10344, #16089, #14807 ) ;
#13684 = EDGE_CURVE ( 'NONE', #6928, #11785, #2003, .T. ) ;
#13685 = CARTESIAN_POINT ( 'NONE',  ( 33.33308377457396432, -5.274811626130743392, -3.627061608673668225 ) ) ;
#13686 = EDGE_CURVE ( 'NONE', #12847, #17090, #8592, .T. ) ;
#13687 = CARTESIAN_POINT ( 'NONE',  ( 28.28955653359400557, -5.882457056865704637, -3.627061608673668225 ) ) ;
#13688 = ORIENTED_EDGE ( 'NONE', *, *, #13782, .T. ) ;
#13689 = CARTESIAN_POINT ( 'NONE',  ( 31.05948030073166066, -1.776715885202022394, 5.783357778048665132 ) ) ;
#13690 = CARTESIAN_POINT ( 'NONE',  ( -20.00000000000000000, 7.999999999999996447, 12.00000000000000000 ) ) ;
#13691 = CIRCLE ( 'NONE', #2684, 11.80000000000000249 ) ;
#13692 = PRESENTATION_LAYER_ASSIGNMENT (  '', '', ( #17506 ) ) ;
#13693 = EDGE_LOOP ( 'NONE', ( #11367, #14491, #14198, #7786 ) ) ;
#13694 = CARTESIAN_POINT ( 'NONE',  ( 32.16857880351144416, -6.669052543620333395, 5.783357778048658915 ) ) ;
#13695 = ADVANCED_FACE ( 'NONE', ( #13853 ), #10030, .T. ) ;
#13696 = CARTESIAN_POINT ( 'NONE',  ( 28.36401332423200827, -6.500457016816879374, -6.861505862736166250 ) ) ;
#13697 = CARTESIAN_POINT ( 'NONE',  ( 25.76524775868381667, -2.816745038626284892, -5.277258820486252944 ) ) ;
#13698 = DIRECTION ( 'NONE',  ( 0.000000000000000000, 0.000000000000000000, -1.000000000000000000 ) ) ;
#13699 = CARTESIAN_POINT ( 'NONE',  ( 28.38593337277646711, -7.124786616671554107, -5.783357778048668685 ) ) ;
#13700 = CYLINDRICAL_SURFACE ( 'NONE', #15098, 3.000000000000000000 ) ;
#13701 = DIRECTION ( 'NONE',  ( -0.1196152422706626278, 0.9928203230275510771, 0.000000000000000000 ) ) ;
#13702 = LINE ( 'NONE', #16691, #12500 ) ;
#13703 = VECTOR ( 'NONE', #16972, 1000.000000000000000 ) ;
#13704 = CARTESIAN_POINT ( 'NONE',  ( 29.86122125502053848, -4.439161430227785310, -8.283357778048662468 ) ) ;
#13705 = ORIENTED_EDGE ( 'NONE', *, *, #6720, .F. ) ;
#13706 = STYLED_ITEM ( 'NONE', ( #3931 ), #17227 ) ;
#13707 = CARTESIAN_POINT ( 'NONE',  ( 33.28924367748503244, -4.026152426421394814, -7.939653947423662039 ) ) ;
#13708 = PRESENTATION_LAYER_ASSIGNMENT (  '', '', ( #11365 ) ) ;
#13709 = DIRECTION ( 'NONE',  ( 1.000000000000000000, 0.000000000000000000, 0.000000000000000000 ) ) ;
#13710 = CARTESIAN_POINT ( 'NONE',  ( 26.53943449477818106, -2.321292140958837624, -6.453230759126469707 ) ) ;
#13711 = DIRECTION ( 'NONE',  ( 0.000000000000000000, 0.000000000000000000, -1.000000000000000000 ) ) ;
#13712 = CARTESIAN_POINT ( 'NONE',  ( 26.31556265977298992, -7.384422263489805793, -5.783357778048663356 ) ) ;
#13713 = EDGE_CURVE ( 'NONE', #1609, #10333, #1630, .T. ) ;
#13714 = CARTESIAN_POINT ( 'NONE',  ( 29.01637427789896151, -7.048830937829682064, -5.783357778048668685 ) ) ;
#13715 = ADVANCED_FACE ( 'NONE', ( #4252 ), #9753, .T. ) ;
#13716 = CARTESIAN_POINT ( 'NONE',  ( -2.016448651773435938E-27, -20.49999999999999645, 6.000000000000000000 ) ) ;
#13717 = CARTESIAN_POINT ( 'NONE',  ( -2.000000000000000444, -3.464101615137763268, -2.842992957459239189 ) ) ;
#13718 = VERTEX_POINT ( 'NONE', #263 ) ;
#13719 = CARTESIAN_POINT ( 'NONE',  ( 30.19827253897071273, -3.144612341114421561, -7.939653947423660263 ) ) ;
#13720 = CARTESIAN_POINT ( 'NONE',  ( 0.000000000000000000, 0.000000000000000000, 0.000000000000000000 ) ) ;
#13721 = CARTESIAN_POINT ( 'NONE',  ( 32.51858583609114106, -1.611119345748072362, -5.783357778048658027 ) ) ;
#13722 = DIRECTION ( 'NONE',  ( -0.000000000000000000, -0.000000000000000000, 1.000000000000000000 ) ) ;
#13723 = CARTESIAN_POINT ( 'NONE',  ( -45.00000000000000711, 0.000000000000000000, -5.537981825772250843 ) ) ;
#13724 = CARTESIAN_POINT ( 'NONE',  ( 33.73390066541284682, -2.518766455766909385, -3.283357778048662023 ) ) ;
#13725 = EDGE_CURVE ( 'NONE', #12534, #3987, #15143, .T. ) ;
#13726 = VERTEX_POINT ( 'NONE', #9456 ) ;
#13727 = CARTESIAN_POINT ( 'NONE',  ( 29.77118727536321074, -5.903822331637461396, -3.283357778048667797 ) ) ;
#13728 = ADVANCED_FACE ( 'NONE', ( #5505 ), #12811, .F. ) ;
#13729 = CARTESIAN_POINT ( 'NONE',  ( 29.77797860222238313, -3.195249460342344250, 7.939653947423664704 ) ) ;
#13730 = DIRECTION ( 'NONE',  ( 0.000000000000000000, 0.000000000000000000, -1.000000000000000000 ) ) ;
#13731 = CARTESIAN_POINT ( 'NONE',  ( -4.211140560182196957, 2.431303136016540911, -3.445885042887435468 ) ) ;
#13732 = EDGE_LOOP ( 'NONE', ( #16085, #7961, #5756, #13541, #16702 ) ) ;
#13733 = CARTESIAN_POINT ( 'NONE',  ( 32.60321786976872005, -6.626883982076972934, -5.783357778048663356 ) ) ;
#13734 = ORIENTED_EDGE ( 'NONE', *, *, #13283, .F. ) ;
#13735 = DIRECTION ( 'NONE',  ( 0.3420201433256631063, 0.000000000000000000, -0.9396926207859104263 ) ) ;
#13736 = EDGE_CURVE ( 'NONE', #7124, #8875, #2687, .T. ) ;
#13737 = EDGE_LOOP ( 'NONE', ( #12348, #12615, #13082 ) ) ;
#13738 = CARTESIAN_POINT ( 'NONE',  ( -35.74085044863416272, -18.73429073671335132, -11.27079897466147607 ) ) ;
#13739 = CARTESIAN_POINT ( 'NONE',  ( 31.44176105920648823, -5.502678662656354192, -3.627061608673668225 ) ) ;
#13740 = UNCERTAINTY_MEASURE_WITH_UNIT (LENGTH_MEASURE( 1.000000000000000082E-05 ), #165, 'distance_accuracy_value', 'NONE');
#13741 = DIRECTION ( 'NONE',  ( 1.000000000000000000, 0.000000000000000000, 0.000000000000000000 ) ) ;
#13742 = CARTESIAN_POINT ( 'NONE',  ( 29.71979337562451207, -1.938121702948446323, 5.783357778048662468 ) ) ;
#13743 = CARTESIAN_POINT ( 'NONE',  ( 23.00000000000000000, -16.21813761408365195, -18.00000000000000355 ) ) ;
#13744 = B_SPLINE_CURVE_WITH_KNOTS ( 'NONE', 3,
 ( #515, #15382, #1523, #1699 ),
 .UNSPECIFIED., .F., .F.,
 ( 4, 4 ),
 ( 0.007932485430080134237, 0.009354825709699442216 ),
 .UNSPECIFIED. ) ;
#13745 = CARTESIAN_POINT ( 'NONE',  ( 26.46816385032927599, -3.594016774262162706, 7.939653947423664704 ) ) ;
#13746 = APPLICATION_CONTEXT ( 'automotive_design' ) ;
#13747 = PRODUCT ( 'BR-592', 'BR-592', '', ( #5769 ) ) ;
#13748 = CARTESIAN_POINT ( 'NONE',  ( 27.71165237056504438, -5.952083095804076684, 3.627061608673662896 ) ) ;
#13749 = EDGE_CURVE ( 'NONE', #11624, #15791, #13404, .T. ) ;
#13750 = CARTESIAN_POINT ( 'NONE',  ( 0.000000000000000000, 0.000000000000000000, 1.599999999999998979 ) ) ;
#13751 = DIRECTION ( 'NONE',  ( 0.000000000000000000, 0.8660254037844380415, -0.5000000000000011102 ) ) ;
#13752 = VERTEX_POINT ( 'NONE', #8122 ) ;
#13753 = ORIENTED_EDGE ( 'NONE', *, *, #2462, .F. ) ;
#13754 = CARTESIAN_POINT ( 'NONE',  ( 32.34358231980129261, -4.140085944684206432, 7.939653947423662039 ) ) ;
#13755 = CARTESIAN_POINT ( 'NONE',  ( 28.52524344760924180, -2.419399995203538101, -7.033357778048658027 ) ) ;
#13756 = ORIENTED_EDGE ( 'NONE', *, *, #4516, .F. ) ;
#13757 = CARTESIAN_POINT ( 'NONE',  ( 29.76058531221316272, -5.705227139567997874, 3.627061608673662896 ) ) ;
#13758 = VERTEX_POINT ( 'NONE', #13656 ) ;
#13759 = DIRECTION ( 'NONE',  ( 0.000000000000000000, 0.000000000000000000, 1.000000000000000000 ) ) ;
#13760 = EDGE_CURVE ( 'NONE', #10596, #1653, #1245, .T. ) ;
#13761 = DIRECTION ( 'NONE',  ( 0.9237280213470681067, 0.3830490080632377170, 0.000000000000000000 ) ) ;
#13762 = CARTESIAN_POINT ( 'NONE',  ( 26.15738093914773543, -4.885401043216321959, -8.283357778048662468 ) ) ;
#13763 = CARTESIAN_POINT ( 'NONE',  ( 0.000000000000000000, 0.000000000000000000, -2.000000000000000000 ) ) ;
#13764 = ORIENTED_EDGE ( 'NONE', *, *, #3519, .T. ) ;
#13765 = CARTESIAN_POINT ( 'NONE',  ( 31.35480929215617252, -6.439933945126671055, -7.033357778048666908 ) ) ;
#13766 = DIRECTION ( 'NONE',  ( 0.9928203230275512992, 0.1196152422706610180, 4.006172263299093133E-17 ) ) ;
#13767 = DIRECTION ( 'NONE',  ( 0.9396926207859104263, 0.000000000000000000, -0.3420201433256631618 ) ) ;
#13768 = CARTESIAN_POINT ( 'NONE',  ( 28.40059689994085801, -13.06564623954105464, 13.61006631438115200 ) ) ;
#13769 = EDGE_LOOP ( 'NONE', ( #2055, #1924, #3255, #1458 ) ) ;
#13770 = EDGE_CURVE ( 'NONE', #6942, #14539, #4708, .T. ) ;
#13771 = CARTESIAN_POINT ( 'NONE',  ( 28.49970350196817392, -5.857138497251738407, -7.939653947423664704 ) ) ;
#13772 = ADVANCED_FACE ( 'NONE', ( #1602 ), #2316, .T. ) ;
#13773 = CARTESIAN_POINT ( 'NONE',  ( 29.76058531221316272, -5.705227139567997874, -7.939653947423662927 ) ) ;
#13774 = ORIENTED_EDGE ( 'NONE', *, *, #3022, .F. ) ;
#13775 = CARTESIAN_POINT ( 'NONE',  ( 3.248936832696172505, -15.16081378324841289, -17.00000000000000000 ) ) ;
#13776 = PLANE ( 'NONE',  #6112 ) ;
#13777 = ORIENTED_EDGE ( 'NONE', *, *, #5069, .T. ) ;
#13778 = ORIENTED_EDGE ( 'NONE', *, *, #14153, .T. ) ;
#13779 = CARTESIAN_POINT ( 'NONE',  ( 27.72904566057427189, -3.442105416578421284, -3.627061608673662896 ) ) ;
#13780 = DIRECTION ( 'NONE',  ( -0.6000000000000001998, -0.7999999999999999334, 0.000000000000000000 ) ) ;
#13781 = CARTESIAN_POINT ( 'NONE',  ( 32.38298487551052318, -4.135338714860305132, -8.283357778048662468 ) ) ;
#13782 = EDGE_CURVE ( 'NONE', #9735, #7756, #1593, .T. ) ;
#13783 = CARTESIAN_POINT ( 'NONE',  ( 33.55383270609817714, -5.448088258586239796, -3.283357778048667797 ) ) ;
#13784 = CARTESIAN_POINT ( 'NONE',  ( 27.47505859511117521, -2.218764776483033163, -5.783357778048658027 ) ) ;
#13785 = CARTESIAN_POINT ( 'NONE',  ( 32.34167700165585302, -2.686501913001913433, 3.283357778048666464 ) ) ;
#13786 = EDGE_CURVE ( 'NONE', #9975, #17674, #5928, .T. ) ;
#13787 = CARTESIAN_POINT ( 'NONE',  ( 23.00000000000000000, -16.21813761408365195, 13.00000000000000178 ) ) ;
#13788 = DIRECTION ( 'NONE',  ( 1.000000000000000000, 0.000000000000000000, 0.000000000000000000 ) ) ;
#13789 = CARTESIAN_POINT ( 'NONE',  ( 28.44643833274707845, -2.428894455266221275, -7.033357778048658027 ) ) ;
#13790 = DIRECTION ( 'NONE',  ( -5.026720092345836698E-22, 4.581671729415424240E-22, -1.000000000000000000 ) ) ;
#13791 = FILL_AREA_STYLE_COLOUR ( '', #12496 ) ;
#13792 = CARTESIAN_POINT ( 'NONE',  ( 0.000000000000000000, 0.000000000000000000, 0.000000000000000000 ) ) ;
#13793 = DIRECTION ( 'NONE',  ( 0.9928203230275512992, 0.1196152422706614898, -0.000000000000000000 ) ) ;
#13794 = DIRECTION ( 'NONE',  ( -0.000000000000000000, -0.000000000000000000, -1.000000000000000000 ) ) ;
#13795 = CARTESIAN_POINT ( 'NONE',  ( 27.49697864365563760, -2.843094376337701679, -6.861505862736159145 ) ) ;
#13796 = ORIENTED_EDGE ( 'NONE', *, *, #8675, .F. ) ;
#13797 = ORIENTED_EDGE ( 'NONE', *, *, #9068, .F. ) ;
#13798 = DIRECTION ( 'NONE',  ( 0.9928203230275510771, 0.1196152422706614621, -0.000000000000000000 ) ) ;
#13799 = CARTESIAN_POINT ( 'NONE',  ( -45.00000000000000711, -16.03270077640482683, -10.53798182577225084 ) ) ;
#13800 = EDGE_LOOP ( 'NONE', ( #5562, #11245, #3794, #12383 ) ) ;
#13801 = EDGE_CURVE ( 'NONE', #17553, #14662, #17386, .T. ) ;
#13802 = CARTESIAN_POINT ( 'NONE',  ( 29.65098506949083301, -2.583579140294649523, -4.705209693361160461 ) ) ;
#13803 = PLANE ( 'NONE',  #7594 ) ;
#13804 = CARTESIAN_POINT ( 'NONE',  ( 26.66770885555339987, -3.370103022578743612, -8.283357778048658915 ) ) ;
#13805 = EDGE_CURVE ( 'NONE', #9359, #6677, #5566, .T. ) ;
#13806 = DIRECTION ( 'NONE',  ( 0.9928203230275510771, 0.1196152422706609902, 4.006172263299092517E-17 ) ) ;
#13807 = CARTESIAN_POINT ( 'NONE',  ( 27.91310269393460430, -7.181753375802955475, -5.783357778048669573 ) ) ;
#13808 = ORIENTED_EDGE ( 'NONE', *, *, #4753, .F. ) ;
#13809 = CARTESIAN_POINT ( 'NONE',  ( 18.90799107099199716, -20.96007437013451380, -15.70102267215298042 ) ) ;
#13810 = CIRCLE ( 'NONE', #14404, 2.749999999999991118 ) ;
#13811 = CARTESIAN_POINT ( 'NONE',  ( 26.49878054387835746, -2.963357534503999968, 6.861505862736166250 ) ) ;
#13812 = CARTESIAN_POINT ( 'NONE',  ( 0.000000000000000000, 0.000000000000000000, 12.00000000000000000 ) ) ;
#13813 = LINE ( 'NONE', #8557, #6916 ) ;
#13814 = ORIENTED_EDGE ( 'NONE', *, *, #4099, .T. ) ;
#13815 = CARTESIAN_POINT ( 'NONE',  ( -27.17934203385504333, -30.00000000000000355, -0.000000000000000000 ) ) ;
#13816 = EDGE_LOOP ( 'NONE', ( #2964, #12574, #5775, #3286 ) ) ;
#13817 = CYLINDRICAL_SURFACE ( 'NONE', #14182, 2.499999999999999112 ) ;
#13818 = ADVANCED_FACE ( 'NONE', ( #2856 ), #1723, .T. ) ;
#13819 = CARTESIAN_POINT ( 'NONE',  ( 33.75714020991769360, -6.487859128256953767, -5.113484796970860558 ) ) ;
#13820 = CARTESIAN_POINT ( 'NONE',  ( 31.45915434921569798, -2.992700983430681028, -7.939653947423660263 ) ) ;
#13821 = CARTESIAN_POINT ( 'NONE',  ( -4.236525418537980592, 2.416953631397924074, -3.451298686683625050 ) ) ;
#13822 = CARTESIAN_POINT ( 'NONE',  ( 30.01512236704901682, -6.601339762873093875, 4.533357778048659803 ) ) ;
#13823 = CARTESIAN_POINT ( 'NONE',  ( 0.000000000000000000, 0.000000000000000000, -9.600000000000001421 ) ) ;
#13824 = EDGE_CURVE ( 'NONE', #16729, #5056, #4892, .T. ) ;
#13825 = CARTESIAN_POINT ( 'NONE',  ( 28.87615734162756453, -4.557842178314484016, 3.627061608673664228 ) ) ;
#13826 = CIRCLE ( 'NONE', #8034, 5.000000000000000000 ) ;
#13827 = CARTESIAN_POINT ( 'NONE',  ( 26.31556265977298992, -7.384422263489805793, -5.783357778048663356 ) ) ;
#13828 = CARTESIAN_POINT ( 'NONE',  ( 32.49625839967270480, -6.639770485940693412, 6.453230759126467042 ) ) ;
#13829 = CARTESIAN_POINT ( 'NONE',  ( 32.70264286945147347, -5.350767304972614546, 7.939653947423658487 ) ) ;
#13830 = ORIENTED_EDGE ( 'NONE', *, *, #2968, .F. ) ;
#13831 = AXIS2_PLACEMENT_3D ( 'NONE', #4534, #8533, #5613 ) ;
#13832 = ORIENTED_EDGE ( 'NONE', *, *, #1656, .F. ) ;
#13833 = CARTESIAN_POINT ( 'NONE',  ( 28.35948656569675919, -3.366149737736551906, 7.939653947423664704 ) ) ;
#13834 = CARTESIAN_POINT ( 'NONE',  ( 26.67454832010805532, -2.305013593294074514, 6.453230759126474148 ) ) ;
#13835 = VERTEX_POINT ( 'NONE', #8383 ) ;
#13836 = CARTESIAN_POINT ( 'NONE',  ( 28.28955653359400557, -5.882457056865704637, 7.939653947423658487 ) ) ;
#13837 =( BOUNDED_CURVE ( )  B_SPLINE_CURVE ( 2, ( #13742, #9721, #9384, #16553, #8381, #9467, #13822, #13567, #4037 ),
 .UNSPECIFIED., .F., .T. ) 
 B_SPLINE_CURVE_WITH_KNOTS ( ( 3, 2, 2, 2, 3 ),
 ( 0.4807692307692307820, 0.4871794871794871695, 0.5000000000000000000, 0.5128205128205127750, 0.5192307692307692735 ),
 .UNSPECIFIED. ) 
 CURVE ( )  GEOMETRIC_REPRESENTATION_ITEM ( )  RATIONAL_B_SPLINE_CURVE ( ( 0.9330127018922194093, 0.9330127018922196314, 1.000000000000000000, 0.8660254037844387076, 1.000000000000000000, 0.8660254037844387076, 1.000000000000000000, 0.9330127018922187432, 0.9330127018922192983 ) ) 
 REPRESENTATION_ITEM ( '' )  );
#13838 = DIRECTION ( 'NONE',  ( 0.9928203230275510771, 0.1196152422706614205, 0.000000000000000000 ) ) ;
#13839 = AXIS2_PLACEMENT_3D ( 'NONE', #14811, #16597, #843 ) ;
#13840 = CARTESIAN_POINT ( 'NONE',  ( 26.01652455409633902, -4.902371455920926380, 5.783357778048663356 ) ) ;
#13841 = ADVANCED_FACE ( 'NONE', ( #16930 ), #4400, .F. ) ;
#13842 = CARTESIAN_POINT ( 'NONE',  ( 25.71748644841968456, -2.420320648352046078, -5.783357778048663356 ) ) ;
#13843 = VECTOR ( 'NONE', #9025, 1000.000000000000114 ) ;
#13844 = CARTESIAN_POINT ( 'NONE',  ( 25.78518620311324838, -3.676302093007511651, -7.939653947423660263 ) ) ;
#13845 = ORIENTED_EDGE ( 'NONE', *, *, #7617, .F. ) ;
#13846 = CARTESIAN_POINT ( 'NONE',  ( 30.06013935859953534, -5.869009311960810216, -8.283357778048662468 ) ) ;
#13847 = DIRECTION ( 'NONE',  ( 0.000000000000000000, -1.000000000000000000, 0.000000000000000000 ) ) ;
#13848 = CARTESIAN_POINT ( 'NONE',  ( 24.63290760229943643, -10.17177306796459035, -14.56289668145355698 ) ) ;
#13849 = CARTESIAN_POINT ( 'NONE',  ( 26.12124691615246874, -10.79952268558355755, 14.20570119594951208 ) ) ;
#13850 = CARTESIAN_POINT ( 'NONE',  ( 29.67743187657054449, -6.342216019229654833, -4.705209693361169343 ) ) ;
#13851 = CARTESIAN_POINT ( 'NONE',  ( 29.04699097144805364, -6.418171698071525100, -4.705209693361169343 ) ) ;
#13852 = ORIENTED_EDGE ( 'NONE', *, *, #9496, .T. ) ;
#13853 = FACE_OUTER_BOUND ( 'NONE', #16985, .T. ) ;
#13854 = AXIS2_PLACEMENT_3D ( 'NONE', #16303, #1409, #13565 ) ;
#13855 = EDGE_CURVE ( 'NONE', #17066, #512, #4129, .T. ) ;
#13856 = CARTESIAN_POINT ( 'NONE',  ( -1.500000000000000000, -10.05532945112458876, -2.666480854966549074 ) ) ;
#13857 = VERTEX_POINT ( 'NONE', #4488 ) ;
#13858 = VERTEX_POINT ( 'NONE', #1412 ) ;
#13859 = CARTESIAN_POINT ( 'NONE',  ( 28.97253418081003673, -5.800171738120336151, 3.627061608673662896 ) ) ;
#13860 = AXIS2_PLACEMENT_3D ( 'NONE', #3074, #9849, #13947 ) ;
#13861 = CARTESIAN_POINT ( 'NONE',  ( 28.69037342443288452, -3.126411886501869741, -3.283357778048662023 ) ) ;
#13862 = CARTESIAN_POINT ( 'NONE',  ( 30.45719375084302527, -1.849279520242854469, 6.453230759126474148 ) ) ;
#13863 = CARTESIAN_POINT ( 'NONE',  ( 32.53688598753899441, -6.297517047505613697, -7.033357778048666908 ) ) ;
#13864 = ADVANCED_FACE ( 'NONE', ( #15464 ), #5654, .F. ) ;
#13865 = CARTESIAN_POINT ( 'NONE',  ( 9.099998387031005720, -19.29508120620799971, -12.00000000000000000 ) ) ;
#13867 = ADVANCED_FACE ( 'NONE', ( #14018 ), #8567, .T. ) ;
#13866 = CARTESIAN_POINT ( 'NONE',  ( 29.62036837594175154, -3.214238380052812261, -3.627061608673662896 ) ) ;
#13868 = CYLINDRICAL_SURFACE ( 'NONE', #10462, 4.000000000000000000 ) ;
#13869 = FACE_BOUND ( 'NONE', #1933, .T. ) ;
#13870 = CIRCLE ( 'NONE', #6046, 9.500000000000001776 ) ;
#13871 = CARTESIAN_POINT ( 'NONE',  ( 27.90727577511918867, -2.156494279411373061, 5.783357778048657138 ) ) ;
#13872 = CARTESIAN_POINT ( 'NONE',  ( 28.75424055680402802, -6.753251120556833520, -7.033357778048666908 ) ) ;
#13873 = CARTESIAN_POINT ( 'NONE',  ( 30.04066231269008469, -3.163601260824890904, -7.939653947423660263 ) ) ;
#13874 = DIRECTION ( 'NONE',  ( -0.000000000000000000, 1.000000000000000000, 1.224646799147353207E-16 ) ) ;
#13875 = FACE_OUTER_BOUND ( 'NONE', #8225, .T. ) ;
#13876 = CARTESIAN_POINT ( 'NONE',  ( -45.00000000000000711, -19.03270077640482683, -10.53798182577225084 ) ) ;
#13877 = CARTESIAN_POINT ( 'NONE',  ( 42.73333828282231650, -6.338146013849483396, -5.783357778048662468 ) ) ;
#13878 = ADVANCED_FACE ( 'NONE', ( #329, #15547, #3129 ), #8663, .T. ) ;
#13879 = CARTESIAN_POINT ( 'NONE',  ( 32.33415724766913257, -1.960501102408027219, 7.033357778048666020 ) ) ;
#13880 = CARTESIAN_POINT ( 'NONE',  ( 28.25893984004492765, -6.513116296623863377, -4.705209693361168455 ) ) ;
#13881 = AXIS2_PLACEMENT_3D ( 'NONE', #13414, #7882, #9229 ) ;
#13882 = EDGE_LOOP ( 'NONE', ( #10987, #15434 ) ) ;
#13883 = EDGE_LOOP ( 'NONE', ( #16075, #1991 ) ) ;
#13884 = CARTESIAN_POINT ( 'NONE',  ( 10.37836969302994028, -0.6704047395399680420, -6.899999999999998579 ) ) ;
#13885 = DIRECTION ( 'NONE',  ( 0.000000000000000000, 0.000000000000000000, 1.000000000000000000 ) ) ;
#13886 = ORIENTED_EDGE ( 'NONE', *, *, #1937, .F. ) ;
#13887 = CONICAL_SURFACE ( 'NONE', #15627, 5.560781378645573980, 1.221730476396047926 ) ;
#13888 = CARTESIAN_POINT ( 'NONE',  ( 29.56783163384821833, -3.220568019956291383, -7.939653947423660263 ) ) ;
#13889 = DIRECTION ( 'NONE',  ( 0.000000000000000000, 1.000000000000000000, 0.000000000000000000 ) ) ;
#13890 = ORIENTED_EDGE ( 'NONE', *, *, #9412, .T. ) ;
#13891 = CARTESIAN_POINT ( 'NONE',  ( 30.25533603959949502, -6.272589980291270351, -6.861505862736166250 ) ) ;
#13892 = DIRECTION ( 'NONE',  ( -0.000000000000000000, -0.000000000000000000, 1.000000000000000000 ) ) ;
#13893 = CARTESIAN_POINT ( 'NONE',  ( 4.204114824917600579, -1.660420935435634737, -3.302147294767050489 ) ) ;
#13894 = CARTESIAN_POINT ( 'NONE',  ( 26.52522735095806894, -6.721994413439005278, -4.705209693361169343 ) ) ;
#13895 = EDGE_CURVE ( 'NONE', #8205, #11419, #9114, .T. ) ;
#13896 = CARTESIAN_POINT ( 'NONE',  ( 17.60442140056922611, -19.37930158608179809, -15.90915821310915135 ) ) ;
#13897 = EDGE_CURVE ( 'NONE', #15676, #7696, #6209, .T. ) ;
#13898 = ORIENTED_EDGE ( 'NONE', *, *, #16971, .T. ) ;
#13899 = CARTESIAN_POINT ( 'NONE',  ( 26.73899421642883567, -2.634607751922174224, 7.033357778048666020 ) ) ;
#13900 = CLOSED_SHELL ( 'NONE', ( #15933, #11745, #11133, #9436 ) ) ;
#13901 = PRESENTATION_LAYER_ASSIGNMENT (  '', '', ( #599 ) ) ;
#13902 = CARTESIAN_POINT ( 'NONE',  ( 27.88665588685489993, -3.423116496867954162, 7.939653947423664704 ) ) ;
#13903 = CARTESIAN_POINT ( 'NONE',  ( -21.62109127008995557, -22.31747812791595464, 15.20678566061929615 ) ) ;
#13904 = DIRECTION ( 'NONE',  ( 0.000000000000000000, 0.000000000000000000, -1.000000000000000000 ) ) ;
#13905 = ADVANCED_FACE ( 'NONE', ( #11727, #17299 ), #10277, .T. ) ;
#13906 = EDGE_LOOP ( 'NONE', ( #17767, #16790, #2433, #12079, #8792, #2243 ) ) ;
#13907 = DIRECTION ( 'NONE',  ( 0.9899494936611662466, 0.1414213562373111965, 0.000000000000000000 ) ) ;
#13908 = VERTEX_POINT ( 'NONE', #15917 ) ;
#13909 = CARTESIAN_POINT ( 'NONE',  ( -21.42601376483257880, 2.765314980223223529, 6.000000000000000000 ) ) ;
#13910 = CARTESIAN_POINT ( 'NONE',  ( 0.000000000000000000, 0.000000000000000000, 1.599999999999998979 ) ) ;
#13911 = CARTESIAN_POINT ( 'NONE',  ( 27.25621498173240198, -3.499072175709823984, -3.627061608673662008 ) ) ;
#13912 = DIRECTION ( 'NONE',  ( 0.9928203230275512992, 0.1196152422706610180, 4.006172263299093133E-17 ) ) ;
#13913 = CARTESIAN_POINT ( 'NONE',  ( -5.500000000000000888, -20.49999999999999645, -13.00000000000000178 ) ) ;
#13914 = PRODUCT_CONTEXT ( 'NONE', #12677, 'mechanical' ) ;
#13915 = CARTESIAN_POINT ( 'NONE',  ( 30.58169613980036772, -2.898544849976259385, -3.283357778048662023 ) ) ;
#13916 = CARTESIAN_POINT ( 'NONE',  ( 28.73594040535616756, -2.066853418799292630, 5.783357778048668685 ) ) ;
#13917 = VECTOR ( 'NONE', #7360, 1000.000000000000000 ) ;
#13918 = CARTESIAN_POINT ( 'NONE',  ( -15.92260893619738837, -28.39189527176317540, 6.000000000000000000 ) ) ;
#13919 = CARTESIAN_POINT ( 'NONE',  ( 26.83664947211162399, -6.984282976826746037, -4.533357778048668685 ) ) ;
#13920 = CARTESIAN_POINT ( 'NONE',  ( 28.93739072872572393, -3.296523698798161650, 3.627061608673666893 ) ) ;
#13921 = EDGE_CURVE ( 'NONE', #2438, #14580, #848, .T. ) ;
#13922 = ORIENTED_EDGE ( 'NONE', *, *, #11694, .T. ) ;
#13923 = VERTEX_POINT ( 'NONE', #11543 ) ;
#13924 = CIRCLE ( 'NONE', #8428, 6.249999999999996447 ) ;
#13925 = ORIENTED_EDGE ( 'NONE', *, *, #12952, .T. ) ;
#13926 = CARTESIAN_POINT ( 'NONE',  ( 30.27725608814395031, -6.896919580145944195, 5.783357778048658027 ) ) ;
#13927 = DIRECTION ( 'NONE',  ( 0.000000000000000000, 0.000000000000000000, -1.000000000000000000 ) ) ;
#13928 = VERTEX_POINT ( 'NONE', #7407 ) ;
#13929 = B_SPLINE_CURVE_WITH_KNOTS ( 'NONE', 3,
 ( #3580, #13266, #5010, #17383, #10445, #581, #6377, #2138 ),
 .UNSPECIFIED., .F., .F.,
 ( 4, 2, 2, 4 ),
 ( 2.465131517309074801E-07, 0.001183067374689863224, 0.001774477805458929370, 0.002365888236227995951 ),
 .UNSPECIFIED. ) ;
#13930 = EDGE_CURVE ( 'NONE', #714, #16745, #15312, .T. ) ;
#13931 = ORIENTED_EDGE ( 'NONE', *, *, #9964, .F. ) ;
#13932 = DIRECTION ( 'NONE',  ( -0.000000000000000000, -0.000000000000000000, 1.000000000000000000 ) ) ;
#13933 = CARTESIAN_POINT ( 'NONE',  ( -4.211140560182196957, -2.431303136016548017, -3.445885042887436356 ) ) ;
#13934 = CARTESIAN_POINT ( 'NONE',  ( 37.96876116389215383, 4.574485896386907058, -2.283357778048670461 ) ) ;
#13935 = CARTESIAN_POINT ( 'NONE',  ( 26.51200394741821498, -4.842675973971495296, -7.939653947423662039 ) ) ;
#13936 = CARTESIAN_POINT ( 'NONE',  ( -10.50000000000000000, 0.000000000000000000, -3.000000000000002665 ) ) ;
#13937 = CARTESIAN_POINT ( 'NONE',  ( 0.000000000000000000, 2.540000000000001368, 1.599999999999999423 ) ) ;
#13938 = CARTESIAN_POINT ( 'NONE',  ( 28.86683379497783264, -7.466592651343750831, -5.783357778048669573 ) ) ;
#13939 = CYLINDRICAL_SURFACE ( 'NONE', #376, 2.749999999999992006 ) ;
#13940 = CARTESIAN_POINT ( 'NONE',  ( 22.22415228291801981, -10.00312865908476567, -15.08655899088414820 ) ) ;
#13941 = CARTESIAN_POINT ( 'NONE',  ( -1.917618200156724081E-28, -7.000000000000001776, -12.00000000000000000 ) ) ;
#13942 = CARTESIAN_POINT ( 'NONE',  ( 32.67202617590239555, -5.981426544730773287, -4.705209693361168455 ) ) ;
#13943 = ORIENTED_EDGE ( 'NONE', *, *, #16776, .F. ) ;
#13944 =( GEOMETRIC_REPRESENTATION_CONTEXT ( 3 ) GLOBAL_UNCERTAINTY_ASSIGNED_CONTEXT ( ( #12441 ) ) GLOBAL_UNIT_ASSIGNED_CONTEXT ( ( #17825, #11128, #16694 ) ) REPRESENTATION_CONTEXT ( 'NONE', 'WORKASPACE' ) );
#13945 = CARTESIAN_POINT ( 'NONE',  ( 29.14753769709988518, -3.271205139184214072, -3.627061608673662008 ) ) ;
#13946 = EDGE_LOOP ( 'NONE', ( #9331, #8950, #2918, #1067 ) ) ;
#13947 = DIRECTION ( 'NONE',  ( 0.000000000000000000, 0.000000000000000000, -1.000000000000000000 ) ) ;
#13948 = VECTOR ( 'NONE', #1285, 1000.000000000000000 ) ;
#13949 = ADVANCED_FACE ( 'NONE', ( #2150 ), #14652, .T. ) ;
#13950 = ORIENTED_EDGE ( 'NONE', *, *, #5702, .F. ) ;
#13951 =( BOUNDED_CURVE ( )  B_SPLINE_CURVE ( 2, ( #10205, #16940, #1974, #5663, #15381, #1613, #1797, #10013, #15474 ),
 .UNSPECIFIED., .F., .T. ) 
 B_SPLINE_CURVE_WITH_KNOTS ( ( 3, 2, 2, 2, 3 ),
 ( 0.2115384615384615641, 0.2179487179487179516, 0.2307692307692307820, 0.2435897435897435848, 0.2500000000000000000 ),
 .UNSPECIFIED. ) 
 CURVE ( )  GEOMETRIC_REPRESENTATION_ITEM ( )  RATIONAL_B_SPLINE_CURVE ( ( 0.9330127018922194093, 0.9330127018922196314, 1.000000000000000000, 0.8660254037844387076, 1.000000000000000000, 0.8660254037844387076, 1.000000000000000000, 0.9330127018922191873, 0.9330127018922194093 ) ) 
 REPRESENTATION_ITEM ( '' )  );
#13952 = ORIENTED_EDGE ( 'NONE', *, *, #13760, .F. ) ;
#13953 = CARTESIAN_POINT ( 'NONE',  ( 27.50150540219088313, -5.977401655418041138, 7.939653947423658487 ) ) ;
#13954 = EDGE_CURVE ( 'NONE', #9735, #14980, #3591, .T. ) ;
#13955 = ORIENTED_EDGE ( 'NONE', *, *, #13123, .F. ) ;
#13956 = APPLICATION_CONTEXT ( 'automotive_design' ) ;
#13957 = FACE_BOUND ( 'NONE', #267, .T. ) ;
#13958 = LINE ( 'NONE', #5687, #16739 ) ;
#13959 = CARTESIAN_POINT ( 'NONE',  ( -6.528882441595574626, 17.18907124314410950, -16.95629972507819971 ) ) ;
#13960 = CARTESIAN_POINT ( 'NONE',  ( 28.56587103547553852, -2.077146556768465047, -5.113484796970851676 ) ) ;
#13961 = CARTESIAN_POINT ( 'NONE',  ( 29.36638131047866196, -1.990897739957422807, -5.783357778048658027 ) ) ;
#13962 = CARTESIAN_POINT ( 'NONE',  ( 32.24155699611449677, -1.634298987580965923, -5.783357778048664244 ) ) ;
#13963 = DIRECTION ( 'NONE',  ( -0.6000000000000000888, 0.7999999999999999334, 0.000000000000000000 ) ) ;
#13964 = AXIS2_PLACEMENT_3D ( 'NONE', #8485, #7135, #333 ) ;
#13965 = AXIS2_PLACEMENT_3D ( 'NONE', #5145, #16236, #10844 ) ;
#13966 = FACE_OUTER_BOUND ( 'NONE', #12724, .T. ) ;
#13967 = ADVANCED_FACE ( 'NONE', ( #3316 ), #502, .T. ) ;
#13968 = CARTESIAN_POINT ( 'NONE',  ( 27.42949161418789572, -3.278323244185609830, -3.283357778048662023 ) ) ;
#13969 = VERTEX_POINT ( 'NONE', #7484 ) ;
#13970 = CARTESIAN_POINT ( 'NONE',  ( 31.51169109130924184, -2.986371343527201905, -3.627061608673662896 ) ) ;
#13971 = CARTESIAN_POINT ( 'NONE',  ( 0.000000000000000000, 0.000000000000000000, 0.000000000000000000 ) ) ;
#13972 = DIRECTION ( 'NONE',  ( -0.000000000000000000, -0.000000000000000000, -1.000000000000000000 ) ) ;
#13973 = CARTESIAN_POINT ( 'NONE',  ( -3.538288549924106796, -15.34800872113743431, -16.99955934415556769 ) ) ;
#13974 = CARTESIAN_POINT ( 'NONE',  ( 30.37838863598085837, -1.858773980305536089, -5.113484796970855228 ) ) ;
#13975 = ADVANCED_FACE ( 'NONE', ( #6390 ), #15643, .T. ) ;
#13976 = CARTESIAN_POINT ( 'NONE',  ( 33.13353876934984754, -5.498725377814142945, 3.283357778048663800 ) ) ;
#13977 = CARTESIAN_POINT ( 'NONE',  ( 27.30005507882132676, -4.747731375419166788, -3.627061608673664672 ) ) ;
#13978 = CIRCLE ( 'NONE', #6466, 2.749999999999988454 ) ;
#13979 = AXIS2_PLACEMENT_3D ( 'NONE', #2250, #2343, #7861 ) ;
#13980 = VECTOR ( 'NONE', #2153, 1000.000000000000114 ) ;
#13981 =( BOUNDED_CURVE ( )  B_SPLINE_CURVE ( 2, ( #6783, #10921, #16487, #4160, #13762, #6862, #12393, #12754, #520 ),
 .UNSPECIFIED., .F., .T. ) 
 B_SPLINE_CURVE_WITH_KNOTS ( ( 3, 2, 2, 2, 3 ),
 ( 0.8653846153846154188, 0.8717948717948718063, 0.8846153846153845812, 0.8974358974358974672, 0.9012882778258578531 ),
 .UNSPECIFIED. ) 
 CURVE ( )  GEOMETRIC_REPRESENTATION_ITEM ( )  RATIONAL_B_SPLINE_CURVE ( ( 0.9330127018922192983, 0.9330127018922198534, 1.000000000000000000, 0.8660254037844387076, 1.000000000000000000, 0.8660254037844387076, 1.000000000000000000, 0.9597425536373320742, 0.9436786787937823107 ) ) 
 REPRESENTATION_ITEM ( '' )  );
#13982 = ORIENTED_EDGE ( 'NONE', *, *, #5609, .F. ) ;
#13983 = EDGE_LOOP ( 'NONE', ( #10877, #6590, #16709, #17556 ) ) ;
#13984 = ORIENTED_EDGE ( 'NONE', *, *, #6976, .F. ) ;
#13985 = CARTESIAN_POINT ( 'NONE',  ( 2.500000000000000000, -1.178949249685213863, 2.042000000000001148 ) ) ;
#13986 = CARTESIAN_POINT ( 'NONE',  ( 29.81239362717914787, -2.264323817775507397, -4.533357778048659803 ) ) ;
#13987 = ORIENTED_EDGE ( 'NONE', *, *, #10576, .T. ) ;
#13988 = CARTESIAN_POINT ( 'NONE',  ( -22.62696978904229184, -9.966234395617776798, -15.00355996101822242 ) ) ;
#13989 = EDGE_LOOP ( 'NONE', ( #12278, #8918, #5391, #10638 ) ) ;
#13990 = CARTESIAN_POINT ( 'NONE',  ( 28.30694982360322953, -3.372479377640031473, -7.939653947423660263 ) ) ;
#13991 = EDGE_CURVE ( 'NONE', #3955, #13298, #683, .T. ) ;
#13992 = CARTESIAN_POINT ( 'NONE',  ( 29.45101334415624095, -7.006662376286320715, -5.783357778048657138 ) ) ;
#13993 =( BOUNDED_CURVE ( )  B_SPLINE_CURVE ( 2, ( #9319, #17437, #10497, #996, #16324, #803, #12127, #17707, #5227 ),
 .UNSPECIFIED., .F., .T. ) 
 B_SPLINE_CURVE_WITH_KNOTS ( ( 3, 2, 2, 2, 3 ),
 ( 0.1346153846153846367, 0.1410256410256410242, 0.1538461538461538547, 0.1666666666666666574, 0.1730769230769231004 ),
 .UNSPECIFIED. ) 
 CURVE ( )  GEOMETRIC_REPRESENTATION_ITEM ( )  RATIONAL_B_SPLINE_CURVE ( ( 0.9330127018922194093, 0.9330127018922196314, 1.000000000000000000, 0.8660254037844387076, 1.000000000000000000, 0.8660254037844387076, 1.000000000000000000, 0.9330127018922190762, 0.9330127018922194093 ) ) 
 REPRESENTATION_ITEM ( '' )  );
#13994 = ORIENTED_EDGE ( 'NONE', *, *, #7842, .F. ) ;
#13995 = CARTESIAN_POINT ( 'NONE',  ( 31.91459173804834748, -5.445711903524953712, -3.627061608673667781 ) ) ;
#13996 = CARTESIAN_POINT ( 'NONE',  ( 31.78252145740879797, -2.026962321187214311, 7.033357778048666020 ) ) ;
#13997 = CARTESIAN_POINT ( 'NONE',  ( 30.96820195323705605, -2.125071739898741097, -7.033357778048658027 ) ) ;
#13998 = CARTESIAN_POINT ( 'NONE',  ( 29.32081432955537537, -3.050456207659999475, -3.283357778048662023 ) ) ;
#13999 = EDGE_CURVE ( 'NONE', #14684, #12285, #4837, .T. ) ;
#14000 = VERTEX_POINT ( 'NONE', #1879 ) ;
#14001 = CARTESIAN_POINT ( 'NONE',  ( 26.10855331130634127, -2.710563430764044490, 7.033357778048666020 ) ) ;
#14002 = CIRCLE ( 'NONE', #16343, 2.749999999999995559 ) ;
#14003 = CARTESIAN_POINT ( 'NONE',  ( 27.89118264539014547, -6.557423775948280742, 4.705209693361159573 ) ) ;
#14004 = CARTESIAN_POINT ( 'NONE',  ( -20.27016866188220945, -21.85533094420792466, 15.46350303853101593 ) ) ;
#14005 = PLANE ( 'NONE',  #9239 ) ;
#14006 = ORIENTED_EDGE ( 'NONE', *, *, #15609, .T. ) ;
#14007 = CARTESIAN_POINT ( 'NONE',  ( 32.30788887834420819, -1.963665922152317833, -7.033357778048658027 ) ) ;
#14008 = ORIENTED_EDGE ( 'NONE', *, *, #1305, .F. ) ;
#14009 = CYLINDRICAL_SURFACE ( 'NONE', #8107, 2.500000000000001776 ) ;
#14010 = ADVANCED_FACE ( 'NONE', ( #4573 ), #14380, .F. ) ;
#14011 = ORIENTED_EDGE ( 'NONE', *, *, #12273, .T. ) ;
#14012 = DIRECTION ( 'NONE',  ( -0.1196152422706620172, 0.9928203230275510771, 0.000000000000000000 ) ) ;
#14013 = ADVANCED_FACE ( 'NONE', ( #3221, #8763 ), #6016, .T. ) ;
#14014 = CARTESIAN_POINT ( 'NONE',  ( 27.75966235412334981, -2.811446176820259879, -4.705209693361160461 ) ) ;
#14015 = CARTESIAN_POINT ( 'NONE',  ( 33.24613200752366282, -6.212066908601060256, -7.033357778048666908 ) ) ;
#14016 = CARTESIAN_POINT ( 'NONE',  ( 20.00000000000000355, 7.999999999999996447, -6.000000000000000000 ) ) ;
#14017 = APPLICATION_PROTOCOL_DEFINITION ( 'draft international standard', 'automotive_design', 1998, #13746 ) ;
#14018 = FACE_OUTER_BOUND ( 'NONE', #4695, .T. ) ;
#14019 = CARTESIAN_POINT ( 'NONE',  ( 33.58707084003705745, -6.498152266226123963, -5.783357778048669573 ) ) ;
#14020 = CARTESIAN_POINT ( 'NONE',  ( 0.2500000000000002220, 0.000000000000000000, 0.000000000000000000 ) ) ;
#14021 = CARTESIAN_POINT ( 'NONE',  ( -4.281152949374567029, -4.203775615332181026, -1.901951201008075243 ) ) ;
#14022 = CARTESIAN_POINT ( 'NONE',  ( 31.67382807612511542, -6.101689702897060030, 4.705209693361159573 ) ) ;
#14023 = ORIENTED_EDGE ( 'NONE', *, *, #12859, .T. ) ;
#14024 = VERTEX_POINT ( 'NONE', #4750 ) ;
#14025 = CARTESIAN_POINT ( 'NONE',  ( 29.60297508593253468, -5.724216059278466773, 3.627061608673662896 ) ) ;
#14026 = DIRECTION ( 'NONE',  ( 0.9928203230275512992, 0.1196152422706607682, -0.000000000000000000 ) ) ;
#14027 = VERTEX_POINT ( 'NONE', #15825 ) ;
#14028 = CARTESIAN_POINT ( 'NONE',  ( 26.39823381822652593, -6.110324093391315436, 7.939653947423658487 ) ) ;
#14029 = CARTESIAN_POINT ( 'NONE',  ( 26.01652455409633902, -4.902371455920926380, -5.783357778048663356 ) ) ;
#14030 = CARTESIAN_POINT ( 'NONE',  ( 26.92924972366625980, -7.310485091653801781, 5.783357778048669573 ) ) ;
#14031 = VERTEX_POINT ( 'NONE', #3399 ) ;
#14032 = CARTESIAN_POINT ( 'NONE',  ( 29.21955148510287614, -5.970283550416647600, 8.283357778048660691 ) ) ;
#14033 = CARTESIAN_POINT ( 'NONE',  ( 1.764121045782362237E-15, 4.736522675502163437, -3.381124513963625233 ) ) ;
#14034 = CARTESIAN_POINT ( 'NONE',  ( 30.42903939560917337, -1.852671564043892660, -5.783357778048658027 ) ) ;
#14036 = EDGE_CURVE ( 'NONE', #15379, #6312, #5459, .T. ) ;
#14035 = CARTESIAN_POINT ( 'NONE',  ( 30.52163964716380917, -2.178873678870954400, -4.533357778048659803 ) ) ;
#14037 = CARTESIAN_POINT ( 'NONE',  ( -3.443595183066686438, -15.28297513750540837, 16.99984776326509106 ) ) ;
#14038 = DIRECTION ( 'NONE',  ( 0.000000000000000000, 0.000000000000000000, 1.000000000000000000 ) ) ;
#14039 = SURFACE_STYLE_USAGE ( .BOTH. , #16954 ) ;
#14040 = CARTESIAN_POINT ( 'NONE',  ( 30.04066231269008469, -3.163601260824890904, -7.939653947423660263 ) ) ;
#14041 = ORIENTED_EDGE ( 'NONE', *, *, #14215, .T. ) ;
#14042 = ADVANCED_FACE ( 'NONE', ( #1123, #10709 ), #3853, .T. ) ;
#14043 = CARTESIAN_POINT ( 'NONE',  ( 27.14244485254070938, -4.766720295129625029, -7.939653947423662039 ) ) ;
#14044 = CARTESIAN_POINT ( 'NONE',  ( -21.42601376483257880, 2.765314980223223529, -6.000000000000000000 ) ) ;
#14045 = VERTEX_POINT ( 'NONE', #2411 ) ;
#14046 = ORIENTED_EDGE ( 'NONE', *, *, #17551, .F. ) ;
#14047 = ORIENTED_EDGE ( 'NONE', *, *, #17557, .F. ) ;
#14048 = CARTESIAN_POINT ( 'NONE',  ( 28.25893984004492765, -6.513116296623863377, 6.861505862736158257 ) ) ;
#14049 = CARTESIAN_POINT ( 'NONE',  ( 26.25801688195511474, -3.619335333876111171, -7.939653947423660263 ) ) ;
#14050 = PLANE ( 'NONE',  #5154 ) ;
#14051 = CARTESIAN_POINT ( 'NONE',  ( 32.22908376348204484, -1.973160382215000785, -7.033357778048658027 ) ) ;
#14052 = CARTESIAN_POINT ( 'NONE',  ( 28.97253418081003673, -5.800171738120336151, -7.939653947423664704 ) ) ;
#14053 = CARTESIAN_POINT ( 'NONE',  ( 31.67744797322171735, -2.039621600994187656, -7.033357778048658027 ) ) ;
#14054 = CARTESIAN_POINT ( 'NONE',  ( 0.000000000000000000, 0.000000000000000000, -1.901951201008075243 ) ) ;
#14055 = EDGE_CURVE ( 'NONE', #17008, #11483, #14987, .T. ) ;
#14056 = DIRECTION ( 'NONE',  ( 1.000000000000000000, 0.000000000000000000, 0.000000000000000000 ) ) ;
#14057 = UNCERTAINTY_MEASURE_WITH_UNIT (LENGTH_MEASURE( 1.000000000000000082E-05 ), #7945, 'distance_accuracy_value', 'NONE');
#14058 = CARTESIAN_POINT ( 'NONE',  ( 28.12379965168153362, -6.829206799398704675, -7.033357778048666908 ) ) ;
#14059 = ORIENTED_EDGE ( 'NONE', *, *, #12835, .F. ) ;
#14060 = CARTESIAN_POINT ( 'NONE',  ( 28.87615734162756453, -4.557842178314484016, -7.939653947423662039 ) ) ;
#14061 = AXIS2_PLACEMENT_3D ( 'NONE', #1411, #13568, #5473 ) ;
#14062 = ADVANCED_FACE ( 'NONE', ( #5021, #16195 ), #6487, .T. ) ;
#14063 = DIRECTION ( 'NONE',  ( -0.1196152422706618645, 0.9928203230275510771, 0.000000000000000000 ) ) ;
#14064 = LINE ( 'NONE', #4623, #14133 ) ;
#14065 = EDGE_CURVE ( 'NONE', #6631, #15247, #13287, .T. ) ;
#14066 =( BOUNDED_CURVE ( )  B_SPLINE_CURVE ( 2, ( #4521, #5960, #10037 ),
 .UNSPECIFIED., .F., .T. ) 
 B_SPLINE_CURVE_WITH_KNOTS ( ( 3, 3 ),
 ( 0.000000000000000000, 1.000000000000000000 ),
 .UNSPECIFIED. ) 
 CURVE ( )  GEOMETRIC_REPRESENTATION_ITEM ( )  RATIONAL_B_SPLINE_CURVE ( ( 0.9436786787937823107, 0.9410169847269389543, 0.9390195162974519505 ) ) 
 REPRESENTATION_ITEM ( '' )  );
#14067 = CARTESIAN_POINT ( 'NONE',  ( 30.44283453230164227, -2.188368138933637574, -4.533357778048659803 ) ) ;
#14068 = CARTESIAN_POINT ( 'NONE',  ( 30.67935139548315604, -7.248220074880824981, 5.783357778048657138 ) ) ;
#14069 = CARTESIAN_POINT ( 'NONE',  ( 26.46816385032927599, -3.594016774262162262, -3.627061608673662896 ) ) ;
#14070 = VERTEX_POINT ( 'NONE', #4020 ) ;
#14071 = CARTESIAN_POINT ( 'NONE',  ( 26.01652455409633902, -4.902371455920926380, 5.783357778048663356 ) ) ;
#14072 = CARTESIAN_POINT ( 'NONE',  ( -10.50000000000000000, 0.000000000000000000, -7.794427190999915211 ) ) ;
#14073 = VERTEX_POINT ( 'NONE', #17496 ) ;
#14074 = CARTESIAN_POINT ( 'NONE',  ( -24.62787796620740011, -10.18046270510853368, -14.56338605435095701 ) ) ;
#14075 = VERTEX_POINT ( 'NONE', #6648 ) ;
#14076 = CARTESIAN_POINT ( 'NONE',  ( 27.67650891848073158, -3.448435056481901295, -7.939653947423660263 ) ) ;
#14077 = ORIENTED_EDGE ( 'NONE', *, *, #2831, .F. ) ;
#14078 = CARTESIAN_POINT ( 'NONE',  ( 31.41114436565740320, -6.133337902414513820, -4.705209693361168455 ) ) ;
#14079 = CARTESIAN_POINT ( 'NONE',  ( 26.31556265977298992, -7.384422263489805793, -5.783357778048663356 ) ) ;
#14080 = DIRECTION ( 'NONE',  ( -0.9928203230275512992, -0.1196152422706610180, -4.006172263299093133E-17 ) ) ;
#14081 = CARTESIAN_POINT ( 'NONE',  ( 33.13353876934984754, -5.498725377814142945, -8.283357778048662468 ) ) ;
#14082 =( BOUNDED_CURVE ( )  B_SPLINE_CURVE ( 2, ( #13305, #4953, #981, #16047, #3277, #885, #15696, #10050, #7269 ),
 .UNSPECIFIED., .F., .T. ) 
 B_SPLINE_CURVE_WITH_KNOTS ( ( 3, 2, 2, 2, 3 ),
 ( 0.1346153846153846367, 0.1410256410256410242, 0.1538461538461538547, 0.1666666666666666574, 0.1730769230769231004 ),
 .UNSPECIFIED. ) 
 CURVE ( )  GEOMETRIC_REPRESENTATION_ITEM ( )  RATIONAL_B_SPLINE_CURVE ( ( 0.9330127018922194093, 0.9330127018922196314, 1.000000000000000000, 0.8660254037844387076, 1.000000000000000000, 0.8660254037844387076, 1.000000000000000000, 0.9330127018922190762, 0.9330127018922194093 ) ) 
 REPRESENTATION_ITEM ( '' )  );
#14083 = CARTESIAN_POINT ( 'NONE',  ( 23.84191717697471091, -22.42419738538529472, -14.74207411150917757 ) ) ;
#14084 = EDGE_LOOP ( 'NONE', ( #7819, #3324, #16827, #9908 ) ) ;
#14085 = CARTESIAN_POINT ( 'NONE',  ( 32.77709966008947617, -5.968767264923789284, 4.705209693361160461 ) ) ;
#14086 = ADVANCED_FACE ( 'NONE', ( #12002, #3760 ), #1222, .T. ) ;
#14087 = CARTESIAN_POINT ( 'NONE',  ( 27.15566825608056689, -6.646038734597135011, 6.861505862736157368 ) ) ;
#14088 = CARTESIAN_POINT ( 'NONE',  ( -18.31859240410168255, -20.37927276054855596, 15.79761704335050077 ) ) ;
#14089 = CARTESIAN_POINT ( 'NONE',  ( 29.91004888286193619, -6.613999042680076990, 7.033357778048657138 ) ) ;
#14090 = B_SPLINE_CURVE_WITH_KNOTS ( 'NONE', 3,
 ( #7317, #12837, #4490, #12645 ),
 .UNSPECIFIED., .F., .F.,
 ( 4, 4 ),
 ( 0.000000000000000000, 0.002452478801916373706 ),
 .UNSPECIFIED. ) ;
#14091 = ORIENTED_EDGE ( 'NONE', *, *, #14055, .T. ) ;
#14092 = CARTESIAN_POINT ( 'NONE',  ( 31.24221605398236079, -5.726592414339752857, 3.283357778048663356 ) ) ;
#14093 = VERTEX_POINT ( 'NONE', #10883 ) ;
#14094 = CARTESIAN_POINT ( 'NONE',  ( 26.66770885555339987, -3.370103022578743612, 3.283357778048666464 ) ) ;
#14095 = ORIENTED_EDGE ( 'NONE', *, *, #13450, .T. ) ;
#14096 = CYLINDRICAL_SURFACE ( 'NONE', #8472, 3.000000000000000000 ) ;
#14097 = CARTESIAN_POINT ( 'NONE',  ( 33.76397967447234549, -5.422769698972272678, -8.283357778048662468 ) ) ;
#14098 = CARTESIAN_POINT ( 'NONE',  ( 32.30788887834420819, -1.963665922152317833, -7.033357778048658027 ) ) ;
#14099 = CARTESIAN_POINT ( 'NONE',  ( 28.13948077428293715, -7.164676150231702678, 5.113484796970851676 ) ) ;
#14100 = ITEM_DEFINED_TRANSFORMATION ( 'NONE', 'NONE', #8847,  #3575 ) ;
#14101 = CARTESIAN_POINT ( 'NONE',  ( -2.016448651773435938E-27, -20.49999999999999645, -12.00000000000000000 ) ) ;
#14102 = VECTOR ( 'NONE', #13445, 1000.000000000000000 ) ;
#14103 = CARTESIAN_POINT ( 'NONE',  ( 32.97211790677835097, -2.610546234160043610, -8.283357778048660691 ) ) ;
#14104 = FACE_OUTER_BOUND ( 'NONE', #17614, .T. ) ;
#14105 = DIRECTION ( 'NONE',  ( -0.000000000000000000, -1.000000000000000000, -0.000000000000000000 ) ) ;
#14106 = CARTESIAN_POINT ( 'NONE',  ( 29.80442540930208750, -6.953886339277345563, 5.783357778048657138 ) ) ;
#14107 = CIRCLE ( 'NONE', #14973, 0.9000000000000003553 ) ;
#14108 = EDGE_CURVE ( 'NONE', #12566, #7917, #10622, .T. ) ;
#14109 = VERTEX_POINT ( 'NONE', #14904 ) ;
#14110 = ORIENTED_EDGE ( 'NONE', *, *, #83, .F. ) ;
#14111 = CARTESIAN_POINT ( 'NONE',  ( 28.98992747081925359, -3.290194058894681639, 7.939653947423664704 ) ) ;
#14112 = CARTESIAN_POINT ( 'NONE',  ( -45.00000000000000711, -19.03270077640483038, 0.5379818257722508434 ) ) ;
#14113 = DIRECTION ( 'NONE',  ( -0.1196152422706599494, 0.9928203230275514102, 0.000000000000000000 ) ) ;
#14114 = ORIENTED_EDGE ( 'NONE', *, *, #17430, .F. ) ;
#14115 = CARTESIAN_POINT ( 'NONE',  ( 27.14244485254070938, -4.766720295129625029, 3.627061608673664228 ) ) ;
#14116 = DIRECTION ( 'NONE',  ( 0.000000000000000000, 1.000000000000000000, 0.000000000000000000 ) ) ;
#14117 = CARTESIAN_POINT ( 'NONE',  ( 27.58784498402260610, -7.231137369010889770, 5.113484796970851676 ) ) ;
#14118 = CARTESIAN_POINT ( 'NONE',  ( 33.21234388421201800, -5.489230917751459771, -8.283357778048664244 ) ) ;
#14119 = CARTESIAN_POINT ( 'NONE',  ( -1.917618200156724081E-28, -7.000000000000001776, 12.00000000000000000 ) ) ;
#14120 = VERTEX_POINT ( 'NONE', #2487 ) ;
#14121 = CARTESIAN_POINT ( 'NONE',  ( 27.95866967485789090, -6.122194908100387245, -3.283357778048667797 ) ) ;
#14122 = AXIS2_PLACEMENT_3D ( 'NONE', #6452, #17554, #7900 ) ;
#14123 = DIRECTION ( 'NONE',  ( -0.000000000000000000, -0.000000000000000000, 1.000000000000000000 ) ) ;
#14124 = CARTESIAN_POINT ( 'NONE',  ( 25.71748644841968456, -2.420320648352046078, 5.783357778048663356 ) ) ;
#14125 = CARTESIAN_POINT ( 'NONE',  ( 30.67110321781257909, -3.087645581983020637, -7.939653947423660263 ) ) ;
#14126 = FACE_OUTER_BOUND ( 'NONE', #10263, .T. ) ;
#14127 = CARTESIAN_POINT ( 'NONE',  ( 27.24942365487322959, -6.207645047004940686, -3.283357778048667797 ) ) ;
#14128 = ADVANCED_FACE ( 'NONE', ( #17667 ), #16283, .F. ) ;
#14129 = EDGE_LOOP ( 'NONE', ( #11696, #15564, #14813, #1102 ) ) ;
#14130 = CONICAL_SURFACE ( 'NONE', #15580, 2.001963570546863025, 0.9599310885968768137 ) ;
#14131 = ORIENTED_EDGE ( 'NONE', *, *, #13770, .F. ) ;
#14132 = CARTESIAN_POINT ( 'NONE',  ( 29.19137779418881351, -4.519864338893556877, 7.939653947423662039 ) ) ;
#14133 = VECTOR ( 'NONE', #1649, 1000.000000000000000 ) ;
#14134 = ORIENTED_EDGE ( 'NONE', *, *, #12851, .T. ) ;
#14135 = CARTESIAN_POINT ( 'NONE',  ( 26.18940839444933033, -6.337336286969802224, -7.823481096485427777 ) ) ;
#14136 = CARTESIAN_POINT ( 'NONE',  ( 33.68326924318660076, -3.978680127145231893, 8.283357778048662468 ) ) ;
#14137 = CARTESIAN_POINT ( 'NONE',  ( 33.10345976029034887, -2.594722134608779207, -3.283357778048662023 ) ) ;
#14138 = CARTESIAN_POINT ( 'NONE',  ( 33.33308377457396432, -5.274811626130743392, -3.627061608673668225 ) ) ;
#14139 = CARTESIAN_POINT ( 'NONE',  ( 26.01652455409633902, -4.902371455920928156, -5.783357778048663356 ) ) ;
#14140 = EDGE_CURVE ( 'NONE', #5981, #9205, #8600, .T. ) ;
#14141 = DIRECTION ( 'NONE',  ( -0.000000000000000000, -0.000000000000000000, -1.000000000000000000 ) ) ;
#14142 = DIRECTION ( 'NONE',  ( 1.000000000000000000, 0.000000000000000000, 0.000000000000000000 ) ) ;
#14143 = DIRECTION ( 'NONE',  ( -0.1196152422706610735, 0.9928203230275511881, 0.000000000000000000 ) ) ;
#14144 = EDGE_LOOP ( 'NONE', ( #15288, #17812, #16566, #11674 ) ) ;
#14145 = CARTESIAN_POINT ( 'NONE',  ( 28.56093688906631911, -4.595820017735426255, -3.627061608673664672 ) ) ;
#14146 = CARTESIAN_POINT ( 'NONE',  ( 30.45719375084302527, -1.849279520242854469, -5.113484796970851676 ) ) ;
#14147 = CARTESIAN_POINT ( 'NONE',  ( 5.237433445017501299, -16.51494876461869410, 16.99438405180048761 ) ) ;
#14148 = PLANE ( 'NONE',  #7208 ) ;
#14149 = CARTESIAN_POINT ( 'NONE',  ( 31.23537658942770889, -6.791681843624433945, -5.113484796970860558 ) ) ;
#14150 = CARTESIAN_POINT ( 'NONE',  ( 29.95125523467787687, -2.974500528818130096, 8.283357778048664244 ) ) ;
#14151 = CARTESIAN_POINT ( 'NONE',  ( 26.01652455409633902, -4.902371455920926380, -5.783357778048663356 ) ) ;
#14152 = AXIS2_PLACEMENT_3D ( 'NONE', #86, #12765, #15402 ) ;
#14153 = EDGE_CURVE ( 'NONE', #15480, #6423, #6080, .T. ) ;
#14154 = VERTEX_POINT ( 'NONE', #9194 ) ;
#14155 = DIRECTION ( 'NONE',  ( 0.1035898384862230515, -0.8598076211353318232, 0.5000000000000001110 ) ) ;
#14156 = AXIS2_PLACEMENT_3D ( 'NONE', #12094, #16543, #3772 ) ;
#14157 = ORIENTED_EDGE ( 'NONE', *, *, #5958, .F. ) ;
#14158 = FACE_OUTER_BOUND ( 'NONE', #9884, .T. ) ;
#14159 = VERTEX_POINT ( 'NONE', #6562 ) ;
#14160 = ADVANCED_FACE ( 'NONE', ( #10797, #16372 ), #17844, .F. ) ;
#14161 = CARTESIAN_POINT ( 'NONE',  ( 26.01652455409633902, -4.902371455920936150, -5.783357778048664244 ) ) ;
#14162 = VECTOR ( 'NONE', #15741, 1000.000000000000227 ) ;
#14163 =( BOUNDED_CURVE ( )  B_SPLINE_CURVE ( 2, ( #14576, #7319, #14296, #12839, #12920, #4669, #13376, #9118, #10548 ),
 .UNSPECIFIED., .F., .T. ) 
 B_SPLINE_CURVE_WITH_KNOTS ( ( 3, 2, 2, 2, 3 ),
 ( 0.4807692307692307820, 0.4871794871794871695, 0.5000000000000000000, 0.5128205128205127750, 0.5192307692307692735 ),
 .UNSPECIFIED. ) 
 CURVE ( )  GEOMETRIC_REPRESENTATION_ITEM ( )  RATIONAL_B_SPLINE_CURVE ( ( 0.9330127018922194093, 0.9330127018922196314, 1.000000000000000000, 0.8660254037844387076, 1.000000000000000000, 0.8660254037844387076, 1.000000000000000000, 0.9330127018922187432, 0.9330127018922192983 ) ) 
 REPRESENTATION_ITEM ( '' )  );
#14164 = ORIENTED_EDGE ( 'NONE', *, *, #14556, .F. ) ;
#14165 = CARTESIAN_POINT ( 'NONE',  ( 30.76748005699505129, -4.329975141788874993, -7.939653947423662039 ) ) ;
#14166 = DIRECTION ( 'NONE',  ( 0.000000000000000000, 0.000000000000000000, 1.000000000000000000 ) ) ;
#14167 = CARTESIAN_POINT ( 'NONE',  ( 29.26075783691881682, -2.330785036554694489, 7.033357778048666020 ) ) ;
#14168 = CARTESIAN_POINT ( 'NONE',  ( 27.48088551392658729, -7.244023872874614689, 5.783357778048669573 ) ) ;
#14169 = EDGE_LOOP ( 'NONE', ( #8367, #6836, #6105, #5807 ) ) ;
#14170 = CARTESIAN_POINT ( 'NONE',  ( 32.57067411085063924, -7.020353038355215070, -5.783357778048669573 ) ) ;
#14171 = CARTESIAN_POINT ( 'NONE',  ( -20.00000000000000355, 7.999999999999996447, 6.000000000000000000 ) ) ;
#14172 = ORIENTED_EDGE ( 'NONE', *, *, #10518, .F. ) ;
#14173 = CARTESIAN_POINT ( 'NONE',  ( 32.04158527077989760, -6.057382223572642665, 6.861505862736158257 ) ) ;
#14174 = EDGE_CURVE ( 'NONE', #9378, #11951, #15044, .T. ) ;
#14175 = CIRCLE ( 'NONE', #12718, 14.00000000000000178 ) ;
#14176 = AXIS2_PLACEMENT_3D ( 'NONE', #3568, #14635, #7289 ) ;
#14177 = CARTESIAN_POINT ( 'NONE',  ( 0.000000000000000000, 0.000000000000000000, 1.599999999999998979 ) ) ;
#14178 = CARTESIAN_POINT ( 'NONE',  ( -16.75000000000000000, -16.63059030033399921, 16.03574476417184869 ) ) ;
#14179 = EDGE_LOOP ( 'NONE', ( #1799, #10984 ) ) ;
#14180 = DIRECTION ( 'NONE',  ( 1.000000000000000000, 0.000000000000000000, 0.000000000000000000 ) ) ;
#14181 = ORIENTED_EDGE ( 'NONE', *, *, #8627, .F. ) ;
#14182 = AXIS2_PLACEMENT_3D ( 'NONE', #9717, #17772, #15095 ) ;
#14183 = CARTESIAN_POINT ( 'NONE',  ( 26.01652455409633902, -4.902371455920926380, 5.783357778048663356 ) ) ;
#14184 = ORIENTED_EDGE ( 'NONE', *, *, #137, .F. ) ;
#14185 = ORIENTED_EDGE ( 'NONE', *, *, #2584, .F. ) ;
#14186 = CARTESIAN_POINT ( 'NONE',  ( 26.63392073224175505, -2.647267031729148012, -7.033357778048658027 ) ) ;
#14187 = CARTESIAN_POINT ( 'NONE',  ( 27.45766530510195835, -4.728742455708699666, -3.627061608673664672 ) ) ;
#14188 = ADVANCED_FACE ( 'NONE', ( #8548, #15527 ), #11066, .F. ) ;
#14189 = CARTESIAN_POINT ( 'NONE',  ( 31.71123609653335507, -2.762457591843783256, -8.283357778048658915 ) ) ;
#14190 = FACE_OUTER_BOUND ( 'NONE', #14273, .T. ) ;
#14191 = CARTESIAN_POINT ( 'NONE',  ( -1.917618200156724081E-28, -7.000000000000001776, -6.000000000000000000 ) ) ;
#14192 = CARTESIAN_POINT ( 'NONE',  ( 28.51709679197739078, -3.347160818026084339, -3.627061608673662008 ) ) ;
#14193 = CARTESIAN_POINT ( 'NONE',  ( 33.56062403295735663, -2.739515387291124426, -3.627061608673662008 ) ) ;
#14194 = LINE ( 'NONE', #1513, #9050 ) ;
#14195 = DIRECTION ( 'NONE',  ( 0.9928203230275512992, 0.1196152422706614898, -0.000000000000000000 ) ) ;
#14196 = CARTESIAN_POINT ( 'NONE',  ( 29.03376756790819613, -4.538853258604016006, 3.627061608673664228 ) ) ;
#14197 = ADVANCED_FACE ( 'NONE', ( #4113 ), #12354, .T. ) ;
#14198 = ORIENTED_EDGE ( 'NONE', *, *, #7265, .F. ) ;
#14199 = CARTESIAN_POINT ( 'NONE',  ( 26.31376129264123165, -7.369470708288995198, 5.576845458699811076 ) ) ;
#14200 = ORIENTED_EDGE ( 'NONE', *, *, #10595, .T. ) ;
#14201 = CARTESIAN_POINT ( 'NONE',  ( 28.75786045390062995, -2.691183018653962034, 4.705209693361167567 ) ) ;
#14202 = FACE_OUTER_BOUND ( 'NONE', #2357, .T. ) ;
#14203 = VECTOR ( 'NONE', #7591, 1000.000000000000000 ) ;
#14204 = ORIENTED_EDGE ( 'NONE', *, *, #15798, .T. ) ;
#14205 = VECTOR ( 'NONE', #10049, 1000.000000000000000 ) ;
#14206 = CARTESIAN_POINT ( 'NONE',  ( 26.39370705969127684, -2.976016814310973313, 4.705209693361168455 ) ) ;
#14207 = ORIENTED_EDGE ( 'NONE', *, *, #10576, .F. ) ;
#14208 = EDGE_LOOP ( 'NONE', ( #1844, #8859, #12495, #10914 ) ) ;
#14209 = CARTESIAN_POINT ( 'NONE',  ( -4.000000000000000000, -2.512220432843121909, -3.169390650195385906 ) ) ;
#14210 = DIRECTION ( 'NONE',  ( 0.6000000000000001998, -0.7999999999999999334, -0.000000000000000000 ) ) ;
#14211 = CARTESIAN_POINT ( 'NONE',  ( 1.391697335622810838, 4.043246145443373685, -3.203898532754367867 ) ) ;
#14212 = CARTESIAN_POINT ( 'NONE',  ( 32.53688598753899441, -6.297517047505613697, -7.033357778048666908 ) ) ;
#14213 = AXIS2_PLACEMENT_3D ( 'NONE', #15519, #12617, #293 ) ;
#14214 = CARTESIAN_POINT ( 'NONE',  ( 25.52694003402523748, -4.961356722058193114, -8.283357778048662468 ) ) ;
#14215 = EDGE_CURVE ( 'NONE', #5422, #496, #10113, .T. ) ;
#14216 =( GEOMETRIC_REPRESENTATION_CONTEXT ( 3 ) GLOBAL_UNCERTAINTY_ASSIGNED_CONTEXT ( ( #7178 ) ) GLOBAL_UNIT_ASSIGNED_CONTEXT ( ( #10875, #16444, #2660 ) ) REPRESENTATION_CONTEXT ( 'NONE', 'WORKASPACE' ) );
#14217 = CYLINDRICAL_SURFACE ( 'NONE', #842, 6.000000000000000888 ) ;
#14218 = DIRECTION ( 'NONE',  ( -0.5000000000000051070, 1.060575238724903217E-16, -0.8660254037844355990 ) ) ;
#14219 = CARTESIAN_POINT ( 'NONE',  ( 30.65370992780335868, -5.597623261208691581, -3.627061608673667781 ) ) ;
#14220 = ORIENTED_EDGE ( 'NONE', *, *, #9883, .F. ) ;
#14221 = CIRCLE ( 'NONE', #10708, 2.749999999999991118 ) ;
#14222 = CARTESIAN_POINT ( 'NONE',  ( 25.78291734803729796, -2.627872734613073913, -5.430426774474530482 ) ) ;
#14223 = VECTOR ( 'NONE', #15719, 1000.000000000000114 ) ;
#14224 = CARTESIAN_POINT ( 'NONE',  ( -35.62429925076629189, -17.76690233603958546, -10.53798182577225084 ) ) ;
#14225 = EDGE_CURVE ( 'NONE', #17548, #10652, #15443, .T. ) ;
#14226 = EDGE_CURVE ( 'NONE', #15670, #13615, #4466, .T. ) ;
#14227 = ORIENTED_EDGE ( 'NONE', *, *, #16240, .T. ) ;
#14228 = VERTEX_POINT ( 'NONE', #6913 ) ;
#14229 = PRODUCT_DEFINITION ( 'UNKNOWN', '', #12947, #1408 ) ;
#14230 = AXIS2_PLACEMENT_3D ( 'NONE', #16408, #6784, #13504 ) ;
#14231 = VERTEX_POINT ( 'NONE', #12538 ) ;
#14232 = CARTESIAN_POINT ( 'NONE',  ( 27.60205212784272177, -2.830435096530727446, 6.861505862736165362 ) ) ;
#14233 = LINE ( 'NONE', #1821, #5011 ) ;
#14234 = DIRECTION ( 'NONE',  ( -1.000000000000000000, -0.000000000000000000, -0.000000000000000000 ) ) ;
#14235 = CARTESIAN_POINT ( 'NONE',  ( 29.79859849048667897, -1.928627242885762705, -5.783357778048664244 ) ) ;
#14236 = CARTESIAN_POINT ( 'NONE',  ( -18.05624385570398260, -20.06430210183123464, -15.83921756800030245 ) ) ;
#14237 = CARTESIAN_POINT ( 'NONE',  ( 33.56515079149260572, -5.873822666371450119, -6.861505862736167138 ) ) ;
#14238 = CARTESIAN_POINT ( 'NONE',  ( 30.08145424927873535, -6.930706697444451336, -5.783357778048663356 ) ) ;
#14239 = DIRECTION ( 'NONE',  ( 0.9899494936611662466, 0.1414213562373111965, 0.000000000000000000 ) ) ;
#14240 = CIRCLE ( 'NONE', #4389, 2.749999999999992895 ) ;
#14241 = FACE_OUTER_BOUND ( 'NONE', #16857, .T. ) ;
#14242 = CARTESIAN_POINT ( 'NONE',  ( -12.26589791205140045, 14.78806204439702121, 16.57179146834700845 ) ) ;
#14243 = EDGE_CURVE ( 'NONE', #8961, #1004, #15241, .T. ) ;
#14244 = TOROIDAL_SURFACE ( 'NONE', #1223, 4.000000000000000000, 0.2500000000000000000 ) ;
#14245 = AXIS2_PLACEMENT_3D ( 'NONE', #12686, #14142, #12780 ) ;
#14246 = VERTEX_POINT ( 'NONE', #17922 ) ;
#14247 = CARTESIAN_POINT ( 'NONE',  ( 26.99805802979993885, -6.665027654307603022, -4.705209693361168455 ) ) ;
#14248 = CARTESIAN_POINT ( 'NONE',  ( 2.540000000000001368, 0.000000000000000000, 1.599999999999998979 ) ) ;
#14249 = CARTESIAN_POINT ( 'NONE',  ( 26.85044460880409645, -7.319979551716484067, -5.783357778048668685 ) ) ;
#14250 = DIRECTION ( 'NONE',  ( -0.000000000000000000, -0.000000000000000000, 1.000000000000000000 ) ) ;
#14251 = CARTESIAN_POINT ( 'NONE',  ( 28.28511899221430070, -4.629050627332469858, 8.283357778048662468 ) ) ;
#14252 = CARTESIAN_POINT ( 'NONE',  ( 29.74110826630370497, -2.999819088432076786, 3.283357778048666464 ) ) ;
#14253 = CARTESIAN_POINT ( 'NONE',  ( 27.10313151398701947, -6.652368374500619908, -6.861505862736166250 ) ) ;
#14254 = VECTOR ( 'NONE', #15064, 1000.000000000000227 ) ;
#14255 = EDGE_LOOP ( 'NONE', ( #4124, #3124, #14041, #1073, #13830 ) ) ;
#14256 = CARTESIAN_POINT ( 'NONE',  ( 31.26353094466156080, -6.788289799823394866, -5.783357778048663356 ) ) ;
#14257 = ORIENTED_EDGE ( 'NONE', *, *, #1804, .T. ) ;
#14258 = AXIS2_PLACEMENT_3D ( 'NONE', #5407, #16411, #6692 ) ;
#14259 = EDGE_LOOP ( 'NONE', ( #7533, #1801, #4111, #13118 ) ) ;
#14260 = DIRECTION ( 'NONE',  ( -0.000000000000000000, -0.000000000000000000, -1.000000000000000000 ) ) ;
#14261 = ORIENTED_EDGE ( 'NONE', *, *, #6372, .F. ) ;
#14262 = DIRECTION ( 'NONE',  ( 0.9928203230275510771, 0.1196152422706614621, -0.000000000000000000 ) ) ;
#14263 = CARTESIAN_POINT ( 'NONE',  ( 27.91310269393460430, -7.181753375802955475, -5.783357778048669573 ) ) ;
#14264 = ADVANCED_FACE ( 'NONE', ( #12709 ), #1579, .F. ) ;
#14265 = CARTESIAN_POINT ( 'NONE',  ( 32.04158527077989760, -6.057382223572642665, -4.705209693361168455 ) ) ;
#14266 = DIRECTION ( 'NONE',  ( 0.1196152422706609902, -0.9928203230275510771, 0.000000000000000000 ) ) ;
#14267 = AXIS2_PLACEMENT_3D ( 'NONE', #5468, #15096, #6842 ) ;
#14268 = DIRECTION ( 'NONE',  ( -0.1196152422706610735, 0.9928203230275511881, 0.000000000000000000 ) ) ;
#14269 = VECTOR ( 'NONE', #15373, 1000.000000000000000 ) ;
#14270 = CARTESIAN_POINT ( 'NONE',  ( 30.49166216014303643, -4.363205751385915931, -8.283357778048662468 ) ) ;
#14271 = AXIS2_PLACEMENT_3D ( 'NONE', #8261, #13711, #2558 ) ;
#14272 = CYLINDRICAL_SURFACE ( 'NONE', #7459, 10.50000000000000000 ) ;
#14273 = EDGE_LOOP ( 'NONE', ( #1719, #7578, #3140 ) ) ;
#14274 = CARTESIAN_POINT ( 'NONE',  ( 33.40301380667672504, -2.758504307001591549, 7.939653947423664704 ) ) ;
#14275 = EDGE_LOOP ( 'NONE', ( #4434, #6047, #14751, #6065, #17220 ) ) ;
#14276 = AXIS2_PLACEMENT_3D ( 'NONE', #11921, #3604, #17593 ) ;
#14277 = AXIS2_PLACEMENT_3D ( 'NONE', #7569, #10355, #5918 ) ;
#14278 = CARTESIAN_POINT ( 'NONE',  ( 31.31418170428987224, -6.782187383561751659, 6.453230759126467042 ) ) ;
#14279 = CARTESIAN_POINT ( 'NONE',  ( -28.39989834181360706, -19.37183319909320645, 13.61025820885934223 ) ) ;
#14280 = DIRECTION ( 'NONE',  ( -1.000000000000000000, 0.000000000000000000, -0.000000000000000000 ) ) ;
#14281 = VERTEX_POINT ( 'NONE', #7199 ) ;
#14282 = AXIS2_PLACEMENT_3D ( 'NONE', #228, #9190, #14567 ) ;
#14283 = CARTESIAN_POINT ( 'NONE',  ( 21.42601376483257880, 2.765314980223224417, 0.000000000000000000 ) ) ;
#14284 = EDGE_LOOP ( 'NONE', ( #6476, #17096, #15266, #10831 ) ) ;
#14285 = CYLINDRICAL_SURFACE ( 'NONE', #5481, 6.000000000000000888 ) ;
#14286 = LINE ( 'NONE', #13099, #7863 ) ;
#14287 = ORIENTED_EDGE ( 'NONE', *, *, #7834, .T. ) ;
#14288 = CARTESIAN_POINT ( 'NONE',  ( 27.46709037723411839, -6.908327297984874882, -4.533357778048668685 ) ) ;
#14289 = EDGE_CURVE ( 'NONE', #9007, #2012, #16627, .T. ) ;
#14290 = CARTESIAN_POINT ( 'NONE',  ( 31.78252145740879797, -2.026962321187214311, -4.533357778048659803 ) ) ;
#14291 = DIRECTION ( 'NONE',  ( -1.000000000000000000, 0.000000000000000000, 0.000000000000000000 ) ) ;
#14292 = APPLICATION_PROTOCOL_DEFINITION ( 'draft international standard', 'automotive_design', 1998, #4811 ) ;
#14293 = CARTESIAN_POINT ( 'NONE',  ( -2.016448651773435938E-27, -20.49999999999999645, 12.00000000000000000 ) ) ;
#14294 = CARTESIAN_POINT ( 'NONE',  ( 33.44685390376565692, -4.007163506710925027, -7.939653947423662039 ) ) ;
#14295 = CARTESIAN_POINT ( 'NONE',  ( -12.50000000000000000, 0.000000000000000000, -8.722503561260788629 ) ) ;
#14296 = CARTESIAN_POINT ( 'NONE',  ( 29.15568435273173264, -2.343444316361667834, 4.533357778048667797 ) ) ;
#14297 = AXIS2_PLACEMENT_3D ( 'NONE', #1546, #8700, #368 ) ;
#14298 = EDGE_CURVE ( 'NONE', #364, #7462, #5764, .T. ) ;
#14299 = CARTESIAN_POINT ( 'NONE',  ( 30.15443244188179150, -1.895953141405084086, 5.783357778048668685 ) ) ;
#14300 = EDGE_CURVE ( 'NONE', #3035, #11992, #8094, .T. ) ;
#14301 = ORIENTED_EDGE ( 'NONE', *, *, #17524, .T. ) ;
#14302 = CARTESIAN_POINT ( 'NONE',  ( 26.23123039439649418, -6.684454722870805554, 7.310947845559079283 ) ) ;
#14303 = ORIENTED_EDGE ( 'NONE', *, *, #10791, .T. ) ;
#14304 = EDGE_CURVE ( 'NONE', #2542, #15022, #1741, .T. ) ;
#14305 = CARTESIAN_POINT ( 'NONE',  ( 26.66961417369883591, -4.823687054261037055, 7.939653947423662039 ) ) ;
#14306 = CARTESIAN_POINT ( 'NONE',  ( 33.40745134805642635, -4.011910736534825439, -3.283357778048664688 ) ) ;
#14307 = CARTESIAN_POINT ( 'NONE',  ( 26.31284730449749532, -7.327874027665321144, -6.311983372246984914 ) ) ;
#14308 = EDGE_LOOP ( 'NONE', ( #5646, #15731, #12843, #7721 ) ) ;
#14309 = DIRECTION ( 'NONE',  ( 0.000000000000000000, 0.000000000000000000, -1.000000000000000000 ) ) ;
#14310 = AXIS2_PLACEMENT_3D ( 'NONE', #6061, #11142, #16711 ) ;
#14311 = LINE ( 'NONE', #7238, #2947 ) ;
#14312 = CARTESIAN_POINT ( 'NONE',  ( 25.95846283556874212, -3.455553161483297053, -8.283357778048660691 ) ) ;
#14313 = ORIENTED_EDGE ( 'NONE', *, *, #7293, .F. ) ;
#14314 = CARTESIAN_POINT ( 'NONE',  ( 26.90793483298706690, -6.248787706170159773, -8.283357778048662468 ) ) ;
#14315 = DIRECTION ( 'NONE',  ( -0.9928203230275510771, -0.1196152422706610735, 0.000000000000000000 ) ) ;
#14316 = CARTESIAN_POINT ( 'NONE',  ( 1.499999999999999778, -9.380831519646861238, -2.000000000000000000 ) ) ;
#14317 =( LENGTH_UNIT ( ) NAMED_UNIT ( * ) SI_UNIT ( .MILLI., .METRE. ) );
#14318 = CARTESIAN_POINT ( 'NONE',  ( 30.62726312072365431, -1.838986382273682718, -5.783357778048658027 ) ) ;
#14319 = EDGE_LOOP ( 'NONE', ( #11028, #3968, #6775, #17434, #4986 ) ) ;
#14320 = ORIENTED_EDGE ( 'NONE', *, *, #8641, .T. ) ;
#14321 = CARTESIAN_POINT ( 'NONE',  ( 23.47400307746859482, -29.47066586337335892, 14.90105725137469506 ) ) ;
#14322 = CARTESIAN_POINT ( 'NONE',  ( 33.21234388421201089, -5.489230917751459771, 3.283357778048663800 ) ) ;
#14323 = ORIENTED_EDGE ( 'NONE', *, *, #14935, .T. ) ;
#14324 = ORIENTED_EDGE ( 'NONE', *, *, #14387, .F. ) ;
#14325 = ORIENTED_EDGE ( 'NONE', *, *, #16269, .F. ) ;
#14326 = EDGE_CURVE ( 'NONE', #10545, #9975, #9795, .T. ) ;
#14327 = DIRECTION ( 'NONE',  ( 0.9928203230275510771, 0.1196152422706609902, 4.006172263299092517E-17 ) ) ;
#14328 = CARTESIAN_POINT ( 'NONE',  ( 32.67619606237177265, -1.592130426037604352, 5.783357778048668685 ) ) ;
#14329 = DIRECTION ( 'NONE',  ( -0.9928203230275514102, -0.1196152422706598939, 0.000000000000000000 ) ) ;
#14330 = CARTESIAN_POINT ( 'NONE',  ( 28.74176732417158320, -7.092112515190875044, -5.783357778048657138 ) ) ;
#14331 = CARTESIAN_POINT ( 'NONE',  ( -17.22607755114822226, -18.63699807132245212, -15.96626374682043981 ) ) ;
#14332 = CARTESIAN_POINT ( 'NONE',  ( 25.71072941247523502, -3.058302133056337357, -4.705209693361161349 ) ) ;
#14333 = CARTESIAN_POINT ( 'NONE',  ( 33.48062616923409962, 0.02583177435455490112, 5.783357778048664244 ) ) ;
#14334 = CARTESIAN_POINT ( 'NONE',  ( 29.21955148510287614, -5.970283550416647600, -3.283357778048667797 ) ) ;
#14335 = DIRECTION ( 'NONE',  ( -0.05980762113533040492, 0.4964101615137757606, -0.8660254037844384856 ) ) ;
#14336 = DIRECTION ( 'NONE',  ( 0.000000000000000000, 0.000000000000000000, -1.000000000000000000 ) ) ;
#14337 = EDGE_LOOP ( 'NONE', ( #11831, #7927, #17199 ) ) ;
#14338 = ORIENTED_EDGE ( 'NONE', *, *, #5837, .T. ) ;
#14339 = CARTESIAN_POINT ( 'NONE',  ( 26.34117031759772942, -2.982346454214467535, -4.705209693361161349 ) ) ;
#14340 = DIRECTION ( 'NONE',  ( -0.000000000000000000, -0.000000000000000000, 1.000000000000000000 ) ) ;
#14341 = CARTESIAN_POINT ( 'NONE',  ( 33.00219691583784964, -5.514549477365426888, -3.283357778048667797 ) ) ;
#14342 = CARTESIAN_POINT ( 'NONE',  ( 26.30654288775393113, -7.309557114202778649, -5.423232652803458009 ) ) ;
#14343 = CARTESIAN_POINT ( 'NONE',  ( 2.345747346278109990, -3.264484291692499873, -0.01223254789874230961 ) ) ;
#14344 = CARTESIAN_POINT ( 'NONE',  ( 28.55151181693415907, -2.416235175459247486, 7.033357778048666020 ) ) ;
#14345 = CARTESIAN_POINT ( 'NONE',  ( 34.23532670761333918, -6.238269840783186027, -9.783357778048662468 ) ) ;
#14346 = ORIENTED_EDGE ( 'NONE', *, *, #7062, .F. ) ;
#14347 = EDGE_CURVE ( 'NONE', #10379, #16771, #2925, .T. ) ;
#14348 = EDGE_CURVE ( 'NONE', #11388, #17192, #3445, .T. ) ;
#14349 = CARTESIAN_POINT ( 'NONE',  ( 27.90727577511918867, -2.156494279411373061, -5.783357778048670461 ) ) ;
#14350 = VERTEX_POINT ( 'NONE', #7386 ) ;
#14351 = CARTESIAN_POINT ( 'NONE',  ( 29.30958546476020743, -4.505622649006972402, -8.283357778048662468 ) ) ;
#14352 = FACE_OUTER_BOUND ( 'NONE', #2515, .T. ) ;
#14353 = CARTESIAN_POINT ( 'NONE',  ( 0.000000000000000000, -2.357898499370431722, 2.818925648462311528E-15 ) ) ;
#14354 = LINE ( 'NONE', #1940, #3448 ) ;
#14355 = CARTESIAN_POINT ( 'NONE',  ( 28.34209327568754233, -5.876127416962207306, -7.939653947423664704 ) ) ;
#14356 = ORIENTED_EDGE ( 'NONE', *, *, #1079, .F. ) ;
#14357 = CARTESIAN_POINT ( 'NONE',  ( 0.000000000000000000, 0.000000000000000000, -2.000000000000000000 ) ) ;
#14358 = CARTESIAN_POINT ( 'NONE',  ( 41.91396146090167463, 0.4627762229654545090, -5.783357778048662468 ) ) ;
#14359 = CARTESIAN_POINT ( 'NONE',  ( 14.00000000000000178, 1.714505518806294835E-15, -8.700000000000001066 ) ) ;
#14360 = CARTESIAN_POINT ( 'NONE',  ( 32.69820532807177216, -4.097360875439379768, -3.283357778048664688 ) ) ;
#14361 = CARTESIAN_POINT ( 'NONE',  ( -34.91600907648203389, -11.88801210197604341, 12.00000000000000000 ) ) ;
#14362 = EDGE_LOOP ( 'NONE', ( #5151, #11081, #8647, #5737 ) ) ;
#14363 = CARTESIAN_POINT ( 'NONE',  ( 31.25770402584614516, -1.763030703431812674, 5.783357778048668685 ) ) ;
#14364 = ORIENTED_EDGE ( 'NONE', *, *, #11480, .F. ) ;
#14365 = EDGE_CURVE ( 'NONE', #2915, #6589, #5968, .T. ) ;
#14366 = ORIENTED_EDGE ( 'NONE', *, *, #16698, .T. ) ;
#14367 = FACE_OUTER_BOUND ( 'NONE', #821, .T. ) ;
#14368 = CARTESIAN_POINT ( 'NONE',  ( 29.25000000000000000, -16.21813761408365195, 13.00000000000000178 ) ) ;
#14369 = DIRECTION ( 'NONE',  ( 1.224646799147353207E-16, -1.000000000000000000, 0.000000000000000000 ) ) ;
#14370 = VERTEX_POINT ( 'NONE', #8826 ) ;
#14371 = CARTESIAN_POINT ( 'NONE',  ( 25.74999999999998934, -16.21813761408365195, 13.00000000000000355 ) ) ;
#14372 = VERTEX_POINT ( 'NONE', #14358 ) ;
#14373 = DIRECTION ( 'NONE',  ( -0.1196152422706610735, 0.9928203230275511881, 0.000000000000000000 ) ) ;
#14374 = CARTESIAN_POINT ( 'NONE',  ( 15.92260893619738837, -28.39189527176317540, 6.000000000000000000 ) ) ;
#14375 = CARTESIAN_POINT ( 'NONE',  ( -35.77680296528374271, -19.03270077640482683, 10.53798182577225084 ) ) ;
#14376 = EDGE_CURVE ( 'NONE', #9029, #15676, #4018, .T. ) ;
#14377 = B_SPLINE_CURVE_WITH_KNOTS ( 'NONE', 3,
 ( #8093, #3662, #13629, #11902, #7831, #8003, #945, #10700, #16100, #9103, #16187, #1215, #2568, #6729, #1035, #16007, #12074, #2315 ),
 .UNSPECIFIED., .F., .F.,
 ( 4, 2, 2, 2, 2, 2, 2, 2, 4 ),
 ( 0.000000000000000000, 0.0005705796246920900351, 0.001141159249384180070, 0.001711738874076270322, 0.002282318498768360140, 0.002852898123460450176, 0.003423477748152541078, 0.003994057372844632414, 0.004564636997536723750 ),
 .UNSPECIFIED. ) ;
#14378 = CARTESIAN_POINT ( 'NONE',  ( 28.67914455963771303, -4.581578327848842669, -8.283357778048662468 ) ) ;
#14379 = PLANE ( 'NONE',  #8994 ) ;
#14380 = CYLINDRICAL_SURFACE ( 'NONE', #11230, 2.000000000000001776 ) ;
#14381 = CARTESIAN_POINT ( 'NONE',  ( 32.07220196432897552, -5.426722983814484813, -3.627061608673668225 ) ) ;
#14382 = DIRECTION ( 'NONE',  ( -0.9928203230275512992, -0.1196152422706610319, -9.614813431917826478E-17 ) ) ;
#14383 = CARTESIAN_POINT ( 'NONE',  ( -36.27615609941022257, -23.17738945083361557, -12.00000000000000000 ) ) ;
#14384 = CARTESIAN_POINT ( 'NONE',  ( 33.48996557372703364, -1.821249024531260696, 4.533357778048667797 ) ) ;
#14385 = EDGE_LOOP ( 'NONE', ( #2105, #88, #1047, #15652, #8392, #15531 ) ) ;
#14386 = CARTESIAN_POINT ( 'NONE',  ( 26.47269060886452507, -6.728324053342490174, -6.861505862736166250 ) ) ;
#14387 = EDGE_CURVE ( 'NONE', #8190, #15002, #12900, .T. ) ;
#14388 = ORIENTED_EDGE ( 'NONE', *, *, #9016, .F. ) ;
#14389 = CARTESIAN_POINT ( 'NONE',  ( 25.83772294520678159, -3.669972453104032084, 7.939653947423664704 ) ) ;
#14390 = LINE ( 'NONE', #13385, #667 ) ;
#14391 = ORIENTED_EDGE ( 'NONE', *, *, #11713, .F. ) ;
#14392 = CARTESIAN_POINT ( 'NONE',  ( 27.85662501549087366, -2.162596695673018043, -5.113484796970851676 ) ) ;
#14393 = DIRECTION ( 'NONE',  ( 0.000000000000000000, 1.000000000000000000, 0.000000000000000000 ) ) ;
#14394 = CARTESIAN_POINT ( 'NONE',  ( 1.750546785592199463E-15, 4.647089433458765129, -3.272167766733383054 ) ) ;
#14395 = DIRECTION ( 'NONE',  ( -0.000000000000000000, -0.000000000000000000, -1.000000000000000000 ) ) ;
#14396 = EDGE_CURVE ( 'NONE', #13000, #2940, #3470, .T. ) ;
#14397 = AXIS2_PLACEMENT_3D ( 'NONE', #13792, #13972, #7092 ) ;
#14398 = CARTESIAN_POINT ( 'NONE',  ( 25.59340017005574097, -5.757764245108966783, -8.283357778048664244 ) ) ;
#14399 = CARTESIAN_POINT ( 'NONE',  ( 27.69265652961275848, -20.36619546179435503, 13.80192434669152490 ) ) ;
#14400 = CARTESIAN_POINT ( 'NONE',  ( 0.000000000000000000, 0.000000000000000000, 0.000000000000000000 ) ) ;
#14401 = FILL_AREA_STYLE ('',( #9937 ) ) ;
#14402 = CARTESIAN_POINT ( 'NONE',  ( 26.84461768998868436, -2.294720455324902542, -5.783357778048658027 ) ) ;
#14403 = VERTEX_POINT ( 'NONE', #8912 ) ;
#14404 = AXIS2_PLACEMENT_3D ( 'NONE', #13193, #17583, #3761 ) ;
#14405 = CARTESIAN_POINT ( 'NONE',  ( 26.14833026707293939, -5.996374093462653931, -8.004211544232147091 ) ) ;
#14406 = CARTESIAN_POINT ( 'NONE',  ( 30.41656616297672500, -2.191532958677927745, 4.533357778048667797 ) ) ;
#14407 = VERTEX_POINT ( 'NONE', #14448 ) ;
#14408 = VECTOR ( 'NONE', #16965, 1000.000000000000000 ) ;
#14409 = ORIENTED_EDGE ( 'NONE', *, *, #12230, .F. ) ;
#14410 = EDGE_CURVE ( 'NONE', #11056, #14154, #12233, .T. ) ;
#14411 = VERTEX_POINT ( 'NONE', #4814 ) ;
#14412 = CARTESIAN_POINT ( 'NONE',  ( 26.46816385032927599, -3.594016774262162262, 7.939653947423662927 ) ) ;
#14413 = CARTESIAN_POINT ( 'NONE',  ( -8.632250723006722026, -18.84644399697197770, -16.84735068286508763 ) ) ;
#14414 =( NAMED_UNIT ( * ) SI_UNIT ( $, .STERADIAN. ) SOLID_ANGLE_UNIT ( ) );
#14415 = AXIS2_PLACEMENT_3D ( 'NONE', #1768, #15904, #17195 ) ;
#14416 = LINE ( 'NONE', #4439, #14408 ) ;
#14417 = CARTESIAN_POINT ( 'NONE',  ( -16.79042544672876858, -17.04069398696883297, -16.02996823657058911 ) ) ;
#14418 = CARTESIAN_POINT ( 'NONE',  ( 32.82963640218302004, -5.962437625020304388, -4.705209693361169343 ) ) ;
#14419 = CARTESIAN_POINT ( 'NONE',  ( -7.511572993685816850E-16, -4.618802153517020059, -3.204271511726792365 ) ) ;
#14420 = LINE ( 'NONE', #634, #10148 ) ;
#14421 = DIRECTION ( 'NONE',  ( 0.000000000000000000, 0.000000000000000000, 1.000000000000000000 ) ) ;
#14422 = FACE_OUTER_BOUND ( 'NONE', #412, .T. ) ;
#14423 = CARTESIAN_POINT ( 'NONE',  ( 28.09001152836988524, -6.106370808549102414, -8.283357778048664244 ) ) ;
#14424 = ORIENTED_EDGE ( 'NONE', *, *, #13824, .F. ) ;
#14425 = EDGE_CURVE ( 'NONE', #14580, #2839, #749, .T. ) ;
#14426 = CARTESIAN_POINT ( 'NONE',  ( 26.86653773853314320, -2.919050055179571945, -6.861505862736159145 ) ) ;
#14427 = CARTESIAN_POINT ( 'NONE',  ( 31.11087420047036289, -5.742416513891037688, -3.283357778048667797 ) ) ;
#14428 = VERTEX_POINT ( 'NONE', #17375 ) ;
#14429 = FACE_OUTER_BOUND ( 'NONE', #14337, .T. ) ;
#14430 = CARTESIAN_POINT ( 'NONE',  ( 28.15758777499317489, -7.552042790248305160, 5.783357778048657138 ) ) ;
#14431 = ADVANCED_FACE ( 'NONE', ( #10437 ), #15997, .T. ) ;
#14432 = ORIENTED_EDGE ( 'NONE', *, *, #2742, .F. ) ;
#14433 = CARTESIAN_POINT ( 'NONE',  ( 26.01652455409633902, -4.902371455920928156, -5.783357778048663356 ) ) ;
#14434 = VECTOR ( 'NONE', #6073, 1000.000000000000114 ) ;
#14435 = CARTESIAN_POINT ( 'NONE',  ( 33.28924367748503244, -4.026152426421394814, -7.939653947423662039 ) ) ;
#14436 = ORIENTED_EDGE ( 'NONE', *, *, #4099, .F. ) ;
#14437 = CARTESIAN_POINT ( 'NONE',  ( 45.00000000000000711, -19.03270077640483038, -5.537981825772250843 ) ) ;
#14438 = CARTESIAN_POINT ( 'NONE',  ( 31.61111609099199171, -1.710254666422835745, -5.783357778048662468 ) ) ;
#14439 = ORIENTED_EDGE ( 'NONE', *, *, #4462, .F. ) ;
#14440 =( BOUNDED_CURVE ( )  B_SPLINE_CURVE ( 3, ( #6036, #17133, #1709, #7337 ),
 .UNSPECIFIED., .F., .T. ) 
 B_SPLINE_CURVE_WITH_KNOTS ( ( 4, 4 ),
 ( 0.000000000000000000, 3.141592653589793116 ),
 .UNSPECIFIED. ) 
 CURVE ( )  GEOMETRIC_REPRESENTATION_ITEM ( )  RATIONAL_B_SPLINE_CURVE ( ( 1.000000000000000000, 0.3333333333333333703, 0.3333333333333333703, 1.000000000000000000 ) ) 
 REPRESENTATION_ITEM ( '' )  );
#14441 = AXIS2_PLACEMENT_3D ( 'NONE', #457, #9855, #7255 ) ;
#14442 = CARTESIAN_POINT ( 'NONE',  ( 27.04606801335823718, -3.524390735323771118, -7.939653947423660263 ) ) ;
#14443 = AXIS2_PLACEMENT_3D ( 'NONE', #7270, #16048, #12883 ) ;
#14444 = CARTESIAN_POINT ( 'NONE',  ( 26.52522735095806894, -6.721994413439005278, -4.705209693361169343 ) ) ;
#14445 = EDGE_CURVE ( 'NONE', #16037, #9754, #12805, .T. ) ;
#14446 = CARTESIAN_POINT ( 'NONE',  ( 28.99445422935450267, -6.424501337975009996, -6.861505862736166250 ) ) ;
#14447 = FACE_BOUND ( 'NONE', #7681, .T. ) ;
#14448 = CARTESIAN_POINT ( 'NONE',  ( 45.50000000000000000, -19.03270077640483038, 2.787981825772258837 ) ) ;
#14449 = CARTESIAN_POINT ( 'NONE',  ( 7.499998387031003411, -20.49508120620799900, -12.00000000000000000 ) ) ;
#14450 = AXIS2_PLACEMENT_3D ( 'NONE', #15492, #12590, #8414 ) ;
#14451 = CARTESIAN_POINT ( 'NONE',  ( 28.60033944477555323, -4.591072787911525843, -8.283357778048662468 ) ) ;
#14452 = CARTESIAN_POINT ( 'NONE',  ( 29.38468146192651886, -6.677295441714964142, -7.033357778048666908 ) ) ;
#14453 = CARTESIAN_POINT ( 'NONE',  ( 30.64918316926811315, -2.463315982128351678, 4.705209693361167567 ) ) ;
#14454 = AXIS2_PLACEMENT_3D ( 'NONE', #2592, #8120, #1241 ) ;
#14455 = EDGE_CURVE ( 'NONE', #5885, #16382, #15619, .T. ) ;
#14456 = PRODUCT_RELATED_PRODUCT_CATEGORY ( 'part', '', ( #8095 ) ) ;
#14457 = ORIENTED_EDGE ( 'NONE', *, *, #3924, .F. ) ;
#14458 = CARTESIAN_POINT ( 'NONE',  ( 30.00264913441657555, -6.940201157507134511, -5.783357778048657138 ) ) ;
#14459 = LINE ( 'NONE', #14559, #17126 ) ;
#14460 = DIRECTION ( 'NONE',  ( 0.000000000000000000, 0.000000000000000000, 1.000000000000000000 ) ) ;
#14461 = VERTEX_POINT ( 'NONE', #7822 ) ;
#14462 = DIRECTION ( 'NONE',  ( -1.000000000000000000, 0.000000000000000000, 0.000000000000000000 ) ) ;
#14463 = VECTOR ( 'NONE', #7577, 1000.000000000000227 ) ;
#14464 = LINE ( 'NONE', #15817, #9599 ) ;
#14465 = CYLINDRICAL_SURFACE ( 'NONE', #6700, 2.499999999999999112 ) ;
#14466 = FACE_OUTER_BOUND ( 'NONE', #14385, .T. ) ;
#14467 = VECTOR ( 'NONE', #11020, 1000.000000000000000 ) ;
#14468 = EDGE_CURVE ( 'NONE', #13537, #3035, #5001, .T. ) ;
#14469 = CARTESIAN_POINT ( 'NONE',  ( 29.62480591732145996, -4.467644809586046151, -3.283357778048664688 ) ) ;
#14470 = CARTESIAN_POINT ( 'NONE',  ( 33.95908713831673964, -3.945449517755637014, 5.783357778048663356 ) ) ;
#14471 = CONTEXT_DEPENDENT_SHAPE_REPRESENTATION ( #6331, #7953 ) ;
#14472 = DIRECTION ( 'NONE',  ( 1.000000000000000000, 0.000000000000000000, -0.000000000000000000 ) ) ;
#14473 = CARTESIAN_POINT ( 'NONE',  ( 29.04699097144805364, -6.418171698071525100, -4.705209693361169343 ) ) ;
#14474 = CARTESIAN_POINT ( 'NONE',  ( -7.374038404636016786, -5.989453865500021124, -2.000000000000000000 ) ) ;
#14475 = DIRECTION ( 'NONE',  ( -0.1196152422706620172, 0.9928203230275510771, 0.000000000000000000 ) ) ;
#14476 = CARTESIAN_POINT ( 'NONE',  ( 28.28955653359400557, -5.882457056865704637, 7.939653947423658487 ) ) ;
#14477 = VECTOR ( 'NONE', #7425, 1000.000000000000227 ) ;
#14478 = AXIS2_PLACEMENT_3D ( 'NONE', #9980, #16715, #1758 ) ;
#14479 = EDGE_LOOP ( 'NONE', ( #4371, #8187, #4722, #15977 ) ) ;
#14480 = CARTESIAN_POINT ( 'NONE',  ( 25.71072941247523502, -3.058302133056337357, -4.705209693361161349 ) ) ;
#14481 = ORIENTED_EDGE ( 'NONE', *, *, #13930, .T. ) ;
#14482 = CARTESIAN_POINT ( 'NONE',  ( 32.18597209352066812, -4.159074864394664672, 3.627061608673664228 ) ) ;
#14483 = CARTESIAN_POINT ( 'NONE',  ( 27.95866967485789090, -6.122194908100387245, 8.283357778048660691 ) ) ;
#14484 = FACE_OUTER_BOUND ( 'NONE', #12826, .T. ) ;
#14485 = EDGE_LOOP ( 'NONE', ( #941, #13630, #3476, #10224 ) ) ;
#14486 = CARTESIAN_POINT ( 'NONE',  ( 27.92107091181166467, -2.492190854301117753, -4.533357778048659803 ) ) ;
#14487 = CARTESIAN_POINT ( 'NONE',  ( 30.32207992551315812, -1.865558067907615802, 5.113484796970859669 ) ) ;
#14488 = CARTESIAN_POINT ( 'NONE',  ( 28.21828588914510050, -7.155181690169023057, -6.453230759126468818 ) ) ;
#14489 = CIRCLE ( 'NONE', #6653, 9.500000000000001776 ) ;
#14490 = CARTESIAN_POINT ( 'NONE',  ( 32.82963640218302004, -5.962437625020304388, -4.705209693361169343 ) ) ;
#14491 = ORIENTED_EDGE ( 'NONE', *, *, #13442, .T. ) ;
#14492 = CARTESIAN_POINT ( 'NONE',  ( 33.60446413004628141, -3.988174587000466342, -3.627061608673664672 ) ) ;
#14493 = CARTESIAN_POINT ( 'NONE',  ( 50.00000000000000000, -16.03270077640482683, 5.537981825772250843 ) ) ;
#14494 = PLANE ( 'NONE',  #6071 ) ;
#14495 = CARTESIAN_POINT ( 'NONE',  ( 29.51982165028991645, -6.361204938940122844, -4.705209693361168455 ) ) ;
#14496 = ORIENTED_EDGE ( 'NONE', *, *, #3384, .F. ) ;
#14497 = AXIS2_PLACEMENT_3D ( 'NONE', #17314, #971, #7947 ) ;
#14498 = EDGE_CURVE ( 'NONE', #2160, #5316, #865, .T. ) ;
#14499 = CARTESIAN_POINT ( 'NONE',  ( 32.33415724766913257, -1.960501102408027219, -4.533357778048659803 ) ) ;
#14500 = CARTESIAN_POINT ( 'NONE',  ( 31.95146207396702565, -5.641142275435198528, 3.283357778048663800 ) ) ;
#14501 = VECTOR ( 'NONE', #17286, 1000.000000000000114 ) ;
#14502 = ORIENTED_EDGE ( 'NONE', *, *, #15609, .F. ) ;
#14503 = AXIS2_PLACEMENT_3D ( 'NONE', #16394, #13751, #2511 ) ;
#14504 = ORIENTED_EDGE ( 'NONE', *, *, #8896, .F. ) ;
#14505 = EDGE_LOOP ( 'NONE', ( #15913, #15650, #10496, #1092 ) ) ;
#14506 = CARTESIAN_POINT ( 'NONE',  ( -3.538288549924106796, -15.34800872113743431, 16.99955934415556769 ) ) ;
#14507 = DIRECTION ( 'NONE',  ( -0.000000000000000000, -0.000000000000000000, -1.000000000000000000 ) ) ;
#14508 = LINE ( 'NONE', #17248, #16456 ) ;
#14509 = CIRCLE ( 'NONE', #7833, 25.00000000000000000 ) ;
#14510 = CYLINDRICAL_SURFACE ( 'NONE', #7529, 2.100000000000000089 ) ;
#14511 = CARTESIAN_POINT ( 'NONE',  ( -22.21647589440744142, -22.43199035874600966, -15.08811024704901094 ) ) ;
#14512 = CARTESIAN_POINT ( 'NONE',  ( 33.56062403295735663, -2.739515387291124426, -3.627061608673662008 ) ) ;
#14513 = FACE_OUTER_BOUND ( 'NONE', #4192, .T. ) ;
#14514 = CARTESIAN_POINT ( 'NONE',  ( 27.58784498402260610, -7.231137369010889770, -6.453230759126474148 ) ) ;
#14515 = CARTESIAN_POINT ( 'NONE',  ( 45.00000000000000711, 0.000000000000000000, 5.537981825772250843 ) ) ;
#14516 = CARTESIAN_POINT ( 'NONE',  ( 27.46709037723411839, -6.908327297984874882, -4.533357778048668685 ) ) ;
#14517 = AXIS2_PLACEMENT_3D ( 'NONE', #741, #8819, #7547 ) ;
#14518 = CARTESIAN_POINT ( 'NONE',  ( 17.93919565825226670, -12.54482367096064621, 15.85739159820981747 ) ) ;
#14519 = PRESENTATION_STYLE_ASSIGNMENT (( #2374 ) ) ;
#14520 = ORIENTED_EDGE ( 'NONE', *, *, #12586, .T. ) ;
#14521 = ORIENTED_EDGE ( 'NONE', *, *, #13684, .T. ) ;
#14522 = EDGE_CURVE ( 'NONE', #512, #11172, #17121, .T. ) ;
#14523 = CARTESIAN_POINT ( 'NONE',  ( 27.50150540219088313, -5.977401655418042914, -3.627061608673667781 ) ) ;
#14524 = CARTESIAN_POINT ( 'NONE',  ( 32.67619606237177265, -1.592130426037604352, -5.783357778048658915 ) ) ;
#14525 = ORIENTED_EDGE ( 'NONE', *, *, #549, .T. ) ;
#14526 = CARTESIAN_POINT ( 'NONE',  ( 25.90899358965569022, -2.397247819800704782, 5.113484796970861446 ) ) ;
#14527 = AXIS2_PLACEMENT_3D ( 'NONE', #8253, #9765, #8522 ) ;
#14528 = CARTESIAN_POINT ( 'NONE',  ( 28.64916707261694384, -6.765910400363817523, 7.033357778048657138 ) ) ;
#14529 = EDGE_CURVE ( 'NONE', #3522, #4898, #7164, .T. ) ;
#14530 = VERTEX_POINT ( 'NONE', #17470 ) ;
#14531 = FACE_OUTER_BOUND ( 'NONE', #6347, .T. ) ;
#14532 = AXIS2_PLACEMENT_3D ( 'NONE', #8424, #12775, #12600 ) ;
#14533 = VECTOR ( 'NONE', #12302, 1000.000000000000114 ) ;
#14534 = CARTESIAN_POINT ( 'NONE',  ( 30.01874226414561875, -2.539271660970221944, -6.861505862736159145 ) ) ;
#14535 = ORIENTED_EDGE ( 'NONE', *, *, #6253, .F. ) ;
#14536 = ADVANCED_FACE ( 'NONE', ( #932, #6468 ), #12258, .T. ) ;
#14537 = FACE_OUTER_BOUND ( 'NONE', #13183, .T. ) ;
#14538 = CARTESIAN_POINT ( 'NONE',  ( 31.63927044622584717, -1.706862622621797110, -5.113484796970854340 ) ) ;
#14539 = VERTEX_POINT ( 'NONE', #9517 ) ;
#14540 = CIRCLE ( 'NONE', #9312, 10.50000000000000000 ) ;
#14541 = CARTESIAN_POINT ( 'NONE',  ( 30.00264913441657555, -6.940201157507134511, -5.783357778048657138 ) ) ;
#14542 = CARTESIAN_POINT ( 'NONE',  ( 27.78610916120306129, -6.570083055755264745, -4.705209693361169343 ) ) ;
#14543 = ORIENTED_EDGE ( 'NONE', *, *, #4199, .T. ) ;
#14544 = CARTESIAN_POINT ( 'NONE',  ( 25.77727942049545717, -5.625018267156629115, -7.939653947423662039 ) ) ;
#14545 = AXIS2_PLACEMENT_3D ( 'NONE', #13934, #7059, #3663 ) ;
#14546 = LINE ( 'NONE', #8735, #14223 ) ;
#14547 = CARTESIAN_POINT ( 'NONE',  ( 27.48088551392658729, -7.244023872874614689, -5.783357778048657138 ) ) ;
#14548 = CARTESIAN_POINT ( 'NONE',  ( 3.540000644887451031, 2.810673041921355697, -3.302142222889115519 ) ) ;
#14549 = CIRCLE ( 'NONE', #2653, 6.000000000000000888 ) ;
#14550 = CARTESIAN_POINT ( 'NONE',  ( 26.66018910156667232, -2.644102211984857842, -4.533357778048659803 ) ) ;
#14551 = CARTESIAN_POINT ( 'NONE',  ( 10.50000000000000000, 1.285879139104720831E-15, -2.000000000000000000 ) ) ;
#14552 = VECTOR ( 'NONE', #7503, 1000.000000000000114 ) ;
#14553 = AXIS2_PLACEMENT_3D ( 'NONE', #9617, #15172, #2752 ) ;
#14554 = VECTOR ( 'NONE', #14630, 1000.000000000000227 ) ;
#14555 =( BOUNDED_CURVE ( )  B_SPLINE_CURVE ( 2, ( #7759, #13291, #14750, #10211, #12755, #5765, #14212, #4682, #4328 ),
 .UNSPECIFIED., .F., .T. ) 
 B_SPLINE_CURVE_WITH_KNOTS ( ( 3, 2, 2, 2, 3 ),
 ( 0.1730769230769231004, 0.1794871794871794879, 0.1923076923076923184, 0.2051282051282051211, 0.2115384615384615641 ),
 .UNSPECIFIED. ) 
 CURVE ( )  GEOMETRIC_REPRESENTATION_ITEM ( )  RATIONAL_B_SPLINE_CURVE ( ( 0.9330127018922194093, 0.9330127018922196314, 1.000000000000000000, 0.8660254037844387076, 1.000000000000000000, 0.8660254037844387076, 1.000000000000000000, 0.9330127018922190762, 0.9330127018922194093 ) ) 
 REPRESENTATION_ITEM ( '' )  );
#14556 = EDGE_CURVE ( 'NONE', #1336, #13453, #14970, .T. ) ;
#14557 = VERTEX_POINT ( 'NONE', #5086 ) ;
#14558 = DIRECTION ( 'NONE',  ( 1.000000000000000000, 0.000000000000000000, 0.000000000000000000 ) ) ;
#14559 = CARTESIAN_POINT ( 'NONE',  ( 25.11802603177690330, -16.03270077640482683, 0.5379818257722508434 ) ) ;
#14560 = CYLINDRICAL_SURFACE ( 'NONE', #1419, 14.00000000000000178 ) ;
#14561 = ORIENTED_EDGE ( 'NONE', *, *, #16719, .F. ) ;
#14562 = APPLICATION_CONTEXT ( 'automotive_design' ) ;
#14563 = DIRECTION ( 'NONE',  ( 0.000000000000000000, 1.000000000000000000, 0.000000000000000000 ) ) ;
#14564 = CARTESIAN_POINT ( 'NONE',  ( 31.86581749455020329, -6.715726164782562790, -5.113484796970860558 ) ) ;
#14565 = PLANE ( 'NONE',  #6716 ) ;
#14566 = CARTESIAN_POINT ( 'NONE',  ( 32.18597209352066812, -4.159074864394664672, -7.939653947423662039 ) ) ;
#14567 = DIRECTION ( 'NONE',  ( 0.000000000000000000, 0.000000000000000000, -1.000000000000000000 ) ) ;
#14568 = ORIENTED_EDGE ( 'NONE', *, *, #13999, .T. ) ;
#14569 = EDGE_CURVE ( 'NONE', #579, #12324, #10686, .T. ) ;
#14570 = CARTESIAN_POINT ( 'NONE',  ( 28.23639288985533824, -7.542548330185622874, -5.783357778048669573 ) ) ;
#14571 = CARTESIAN_POINT ( 'NONE',  ( -37.55714628004649569, -12.56174331051002113, -5.783357778048663356 ) ) ;
#14572 = ITEM_DEFINED_TRANSFORMATION ( 'NONE', 'NONE', #9382,  #3575 ) ;
#14573 = CARTESIAN_POINT ( 'NONE',  ( -25.11802603177690330, -16.03270077640482683, -0.5379818257722508434 ) ) ;
#14574 = CARTESIAN_POINT ( 'NONE',  ( 28.93739072872572393, -3.296523698798161650, -7.939653947423660263 ) ) ;
#14575 = CARTESIAN_POINT ( 'NONE',  ( 26.31284730449749532, -7.327874027665321144, -6.311983372246984914 ) ) ;
#14576 = CARTESIAN_POINT ( 'NONE',  ( 29.16815758536418102, -2.004582921727632971, 5.783357778048662468 ) ) ;
#14577 = CARTESIAN_POINT ( 'NONE',  ( 25.88156304229571703, -4.918631652813365562, 3.627061608673664228 ) ) ;
#14578 = ORIENTED_EDGE ( 'NONE', *, *, #5256, .F. ) ;
#14579 = VECTOR ( 'NONE', #583, 1000.000000000000114 ) ;
#14580 = VERTEX_POINT ( 'NONE', #10866 ) ;
#14581 = CARTESIAN_POINT ( 'NONE',  ( 26.13631296615020361, -5.896629108145334364, 7.834650323883576739 ) ) ;
#14582 =( BOUNDED_CURVE ( )  B_SPLINE_CURVE ( 2, ( #14735, #11997, #2048, #9108, #4831, #8925, #9017, #678, #16012 ),
 .UNSPECIFIED., .F., .T. ) 
 B_SPLINE_CURVE_WITH_KNOTS ( ( 3, 2, 2, 2, 3 ),
 ( 0.09615384615384617306, 0.1025641025641025605, 0.1153846153846153910, 0.1282051282051281937, 0.1346153846153846367 ),
 .UNSPECIFIED. ) 
 CURVE ( )  GEOMETRIC_REPRESENTATION_ITEM ( )  RATIONAL_B_SPLINE_CURVE ( ( 0.9330127018922194093, 0.9330127018922196314, 1.000000000000000000, 0.8660254037844387076, 1.000000000000000000, 0.8660254037844387076, 1.000000000000000000, 0.9330127018922190762, 0.9330127018922194093 ) ) 
 REPRESENTATION_ITEM ( '' )  );
#14583 = ORIENTED_EDGE ( 'NONE', *, *, #16289, .T. ) ;
#14584 = EDGE_CURVE ( 'NONE', #14159, #4061, #2537, .T. ) ;
#14585 = CARTESIAN_POINT ( 'NONE',  ( 25.72395281601508898, -4.937620572523835349, 3.627061608673664228 ) ) ;
#14586 = CARTESIAN_POINT ( 'NONE',  ( -29.03633718710667466, -14.58471626061076520, 13.43311195353574305 ) ) ;
#14587 = DIRECTION ( 'NONE',  ( -1.000000000000000000, -1.224646799147353454E-16, 0.000000000000000000 ) ) ;
#14588 = EDGE_CURVE ( 'NONE', #1845, #12756, #1015, .T. ) ;
#14589 = ORIENTED_EDGE ( 'NONE', *, *, #12227, .T. ) ;
#14590 = DIRECTION ( 'NONE',  ( 0.000000000000000000, 0.000000000000000000, 1.000000000000000000 ) ) ;
#14591 = DIRECTION ( 'NONE',  ( 0.000000000000000000, 0.000000000000000000, -1.000000000000000000 ) ) ;
#14593 = CIRCLE ( 'NONE', #7053, 5.000000000000000888 ) ;
#14592 = CARTESIAN_POINT ( 'NONE',  ( 27.90727577511918867, -2.156494279411373061, -5.783357778048670461 ) ) ;
#14594 = CARTESIAN_POINT ( 'NONE',  ( 33.30663696749426350, -1.516174747195733863, -5.783357778048658027 ) ) ;
#14595 = CARTESIAN_POINT ( 'NONE',  ( 31.71314141467879111, -4.216041623526076698, -3.627061608673664672 ) ) ;
#14596 = FACE_OUTER_BOUND ( 'NONE', #13462, .T. ) ;
#14597 = CARTESIAN_POINT ( 'NONE',  ( 3.538288549924106796, -15.34800872113743431, 13.00000000000000178 ) ) ;
#14598 =( LENGTH_UNIT ( ) NAMED_UNIT ( * ) SI_UNIT ( .MILLI., .METRE. ) );
#14599 = CARTESIAN_POINT ( 'NONE',  ( 28.12741954877813555, -2.767138697495831856, -6.861505862736159145 ) ) ;
#14600 = CARTESIAN_POINT ( 'NONE',  ( 27.99987602667382802, -2.482696394238434578, 7.033357778048666020 ) ) ;
#14601 = CARTESIAN_POINT ( 'NONE',  ( 30.45035428628836627, -2.914368949527523789, 3.283357778048666464 ) ) ;
#14602 = ORIENTED_EDGE ( 'NONE', *, *, #4934, .F. ) ;
#14603 = ORIENTED_EDGE ( 'NONE', *, *, #13749, .F. ) ;
#14604 = CARTESIAN_POINT ( 'NONE',  ( 30.35023428074701002, -1.862166024106576057, 5.783357778048662468 ) ) ;
#14605 = DIRECTION ( 'NONE',  ( 0.000000000000000000, 0.000000000000000000, -1.000000000000000000 ) ) ;
#14606 = EDGE_CURVE ( 'NONE', #7303, #7229, #13256, .T. ) ;
#14607 = CARTESIAN_POINT ( 'NONE',  ( 29.47916769939009285, -7.003270332485284300, -6.453230759126468818 ) ) ;
#14608 = CARTESIAN_POINT ( 'NONE',  ( -20.83887142315839469, -22.08617648736154493, -15.35754594250728999 ) ) ;
#14609 = CARTESIAN_POINT ( 'NONE',  ( 29.65098506949083301, -2.583579140294649523, -4.705209693361160461 ) ) ;
#14610 = CARTESIAN_POINT ( 'NONE',  ( 19.43845002722867221, 2.988003976273735596, 6.000000000000000000 ) ) ;
#14611 = DIRECTION ( 'NONE',  ( -0.000000000000000000, -0.000000000000000000, -1.000000000000000000 ) ) ;
#14612 = CARTESIAN_POINT ( 'NONE',  ( 32.27410075503257758, -1.240829931302721345, -5.783357778048658027 ) ) ;
#14613 = DIRECTION ( 'NONE',  ( 1.000000000000000000, 0.000000000000000000, 0.000000000000000000 ) ) ;
#14614 = DIRECTION ( 'NONE',  ( 0.1196152422706587976, -0.9928203230275515212, 1.866876274697368064E-15 ) ) ;
#14615 = ADVANCED_FACE ( 'NONE', ( #1025 ), #6547, .F. ) ;
#14616 = ADVANCED_BREP_SHAPE_REPRESENTATION ( '', ( #17490, #3575 ), #11602 ) ;
#14617 = CARTESIAN_POINT ( 'NONE',  ( 26.47269060886452507, -6.728324053342490174, -6.861505862736166250 ) ) ;
#14618 = CARTESIAN_POINT ( 'NONE',  ( 32.69811611091622439, -2.216460025892273311, -6.861505862736158257 ) ) ;
#14619 = ORIENTED_EDGE ( 'NONE', *, *, #4069, .F. ) ;
#14620 = CARTESIAN_POINT ( 'NONE',  ( 3.999999999999999112, 0.000000000000000000, 1.599999999999998979 ) ) ;
#14621 = CARTESIAN_POINT ( 'NONE',  ( 26.24565837299761739, -7.163851760794091916, 4.332150178794286433 ) ) ;
#14622 = ORIENTED_EDGE ( 'NONE', *, *, #182, .T. ) ;
#14623 = CARTESIAN_POINT ( 'NONE',  ( 32.34851646621051202, -1.621412483717243447, -5.113484796970854340 ) ) ;
#14624 = CARTESIAN_POINT ( 'NONE',  ( 32.51858583609114106, -1.611119345748072362, -5.783357778048658915 ) ) ;
#14625 = ORIENTED_EDGE ( 'NONE', *, *, #1056, .F. ) ;
#14626 = EDGE_CURVE ( 'NONE', #2500, #6811, #5797, .T. ) ;
#14627 = CARTESIAN_POINT ( 'NONE',  ( 29.18947247604338102, -3.066280307211263434, -8.283357778048660691 ) ) ;
#14628 = CARTESIAN_POINT ( 'NONE',  ( 26.08205926866327218, -5.446317154234562530, -8.158109112226842541 ) ) ;
#14629 = CARTESIAN_POINT ( 'NONE',  ( 10.50000000000000000, 1.285879139104720831E-15, -7.794427190999915211 ) ) ;
#14630 = DIRECTION ( 'NONE',  ( 0.9928203230275510771, 0.1196152422706614621, -0.000000000000000000 ) ) ;
#14631 = CARTESIAN_POINT ( 'NONE',  ( 33.32864623319426300, -4.021405196597508613, -3.283357778048664688 ) ) ;
#14632 = ADVANCED_FACE ( 'NONE', ( #8343, #13875 ), #1462, .T. ) ;
#14633 = CARTESIAN_POINT ( 'NONE',  ( 27.09860475545177039, -3.518061095420291995, -3.627061608673662896 ) ) ;
#14634 = CARTESIAN_POINT ( 'NONE',  ( 26.30654288775393113, -7.309557114202778649, -5.423232652803458009 ) ) ;
#14635 = DIRECTION ( 'NONE',  ( 0.7020299829125996594, 0.08458074894285609602, -0.7071067811865479058 ) ) ;
#14636 = CARTESIAN_POINT ( 'NONE',  ( 2.742797192660275662, 3.035247456002220900, -3.133250573521050519 ) ) ;
#14637 = CARTESIAN_POINT ( 'NONE',  ( 28.72045243349238675, -6.030415129707233035, -8.283357778048662468 ) ) ;
#14638 = CARTESIAN_POINT ( 'NONE',  ( 30.76748005699505129, -4.329975141788874993, -7.939653947423662039 ) ) ;
#14639 = ORIENTED_EDGE ( 'NONE', *, *, #8818, .F. ) ;
#14640 = CARTESIAN_POINT ( 'NONE',  ( 29.25000000000000000, -16.21813761408365195, 13.37255996287876236 ) ) ;
#14641 = CARTESIAN_POINT ( 'NONE',  ( 29.89119874204131122, -2.254829357712824667, -4.533357778048659803 ) ) ;
#14642 = CARTESIAN_POINT ( 'NONE',  ( 20.00000000000000000, 7.999999999999996447, -12.00000000000000000 ) ) ;
#14643 = ORIENTED_EDGE ( 'NONE', *, *, #3636, .T. ) ;
#14644 = CARTESIAN_POINT ( 'NONE',  ( -4.000000000000000000, 4.898587196589412829E-16, 13.31572692736085095 ) ) ;
#14645 = CARTESIAN_POINT ( 'NONE',  ( 31.21213704492286212, -2.822589171134389563, -3.283357778048662023 ) ) ;
#14646 = LINE ( 'NONE', #3392, #16576 ) ;
#14647 = CARTESIAN_POINT ( 'NONE',  ( 31.54230778485832332, -2.355712103769039611, -4.705209693361160461 ) ) ;
#14648 = CARTESIAN_POINT ( 'NONE',  ( 29.81991338116587542, -2.990324628369393611, 3.283357778048666464 ) ) ;
#14649 = CARTESIAN_POINT ( 'NONE',  ( 29.42969845347704450, -5.944964990802679594, -8.283357778048662468 ) ) ;
#14650 = CARTESIAN_POINT ( 'NONE',  ( -3.510273485745307731, -2.827716139362665082, -3.310536846335889738 ) ) ;
#14651 = B_SPLINE_CURVE_WITH_KNOTS ( 'NONE', 3,
 ( #4725, #17559, #1016, #16165, #14628, #2208, #15988, #13071, #5077, #16080, #17176, #3559, #7642, #13247, #10248, #10598, #10332, #656 ),
 .UNSPECIFIED., .F., .F.,
 ( 4, 2, 2, 2, 2, 2, 2, 2, 4 ),
 ( 0.000000000000000000, 0.0005705796246920901435, 0.001141159249384180287, 0.001711738874076270539, 0.002282318498768360574, 0.002852898123460450609, 0.003423477748152541078, 0.003994057372844630679, 0.004564636997536721148 ),
 .UNSPECIFIED. ) ;
#14652 = CYLINDRICAL_SURFACE ( 'NONE', #1432, 2.500000000000001776 ) ;
#14653 = DIRECTION ( 'NONE',  ( 0.000000000000000000, -1.000000000000000000, 0.000000000000000000 ) ) ;
#14654 = CARTESIAN_POINT ( 'NONE',  ( 31.41531425212677675, -1.744041783721344219, -5.783357778048658027 ) ) ;
#14655 = EDGE_CURVE ( 'NONE', #11687, #2087, #9724, .T. ) ;
#14656 = DIRECTION ( 'NONE',  ( 0.000000000000000000, 0.000000000000000000, 1.000000000000000000 ) ) ;
#14657 = CARTESIAN_POINT ( 'NONE',  ( 33.60446413004628141, -3.988174587000466342, 7.939653947423662039 ) ) ;
#14658 = CARTESIAN_POINT ( 'NONE',  ( 27.02414796481377124, -2.900061135469103490, 4.705209693361168455 ) ) ;
#14659 =( BOUNDED_CURVE ( )  B_SPLINE_CURVE ( 2, ( #4995, #11704, #12057, #17561, #7551, #2123, #4810, #11791, #14541 ),
 .UNSPECIFIED., .F., .T. ) 
 B_SPLINE_CURVE_WITH_KNOTS ( ( 3, 2, 2, 2, 3 ),
 ( 0.4807692307692307820, 0.4871794871794871695, 0.5000000000000000000, 0.5128205128205127750, 0.5192307692307692735 ),
 .UNSPECIFIED. ) 
 CURVE ( )  GEOMETRIC_REPRESENTATION_ITEM ( )  RATIONAL_B_SPLINE_CURVE ( ( 0.9330127018922194093, 0.9330127018922196314, 1.000000000000000000, 0.8660254037844387076, 1.000000000000000000, 0.8660254037844387076, 1.000000000000000000, 0.9330127018922187432, 0.9330127018922192983 ) ) 
 REPRESENTATION_ITEM ( '' )  );
#14660 = ORIENTED_EDGE ( 'NONE', *, *, #686, .F. ) ;
#14661 = DIRECTION ( 'NONE',  ( -0.9979201627913403261, 0.06446199418653535129, 0.000000000000000000 ) ) ;
#14662 = VERTEX_POINT ( 'NONE', #9774 ) ;
#14663 = CARTESIAN_POINT ( 'NONE',  ( 26.23609683341064525, -2.995005734021441768, 4.705209693361167567 ) ) ;
#14664 = CARTESIAN_POINT ( 'NONE',  ( 13.00000000000000178, 0.000000000000000000, 8.700000000000001066 ) ) ;
#14665 = DIRECTION ( 'NONE',  ( 1.000000000000000000, 0.000000000000000000, 0.000000000000000000 ) ) ;
#14666 = EDGE_CURVE ( 'NONE', #475, #6735, #12059, .T. ) ;
#14667 = ORIENTED_EDGE ( 'NONE', *, *, #15520, .F. ) ;
#14668 = LINE ( 'NONE', #8858, #689 ) ;
#14669 = CARTESIAN_POINT ( 'NONE',  ( 2.500000000000000000, 2.357898499370432166, -2.385244779468109755E-15 ) ) ;
#14670 = CARTESIAN_POINT ( 'NONE',  ( 27.89480254248674740, -2.495355674045408367, -7.033357778048658027 ) ) ;
#14671 = CARTESIAN_POINT ( 'NONE',  ( 32.17274868998081416, -2.279756424927169345, -4.705209693361160461 ) ) ;
#14672 = CARTESIAN_POINT ( 'NONE',  ( 32.16857880351144416, -6.669052543620333395, -5.783357778048668685 ) ) ;
#14673 = FACE_OUTER_BOUND ( 'NONE', #872, .T. ) ;
#14674 = CARTESIAN_POINT ( 'NONE',  ( 31.83134908525019213, -4.201799933639492224, -8.283357778048662468 ) ) ;
#14675 = CARTESIAN_POINT ( 'NONE',  ( 27.75549246765397271, -7.200742295513423485, -5.783357778048668685 ) ) ;
#14676 = ADVANCED_FACE ( 'NONE', ( #5527 ), #2738, .F. ) ;
#14677 = FACE_OUTER_BOUND ( 'NONE', #13134, .T. ) ;
#14678 = LINE ( 'NONE', #5889, #11805 ) ;
#14679 = CARTESIAN_POINT ( 'NONE',  ( -9.099998387031003944, -19.29508120620799616, 16.81964500401478091 ) ) ;
#14680 = CARTESIAN_POINT ( 'NONE',  ( 31.20090818012769773, -4.277755612481361602, 3.283357778048664244 ) ) ;
#14681 =( BOUNDED_CURVE ( )  B_SPLINE_CURVE ( 2, ( #17054, #12678, #9758, #4607, #15226, #10036, #4258, #15313, #2803 ),
 .UNSPECIFIED., .F., .T. ) 
 B_SPLINE_CURVE_WITH_KNOTS ( ( 3, 2, 2, 2, 3 ),
 ( 0.2884615384615384914, 0.2948717948717948789, 0.3076923076923077094, 0.3205128205128205399, 0.3269230769230769273 ),
 .UNSPECIFIED. ) 
 CURVE ( )  GEOMETRIC_REPRESENTATION_ITEM ( )  RATIONAL_B_SPLINE_CURVE ( ( 0.9330127018922194093, 0.9330127018922196314, 1.000000000000000000, 0.8660254037844387076, 1.000000000000000000, 0.8660254037844387076, 1.000000000000000000, 0.9330127018922194093, 0.9330127018922194093 ) ) 
 REPRESENTATION_ITEM ( '' )  );
#14682 = ORIENTED_EDGE ( 'NONE', *, *, #17531, .T. ) ;
#14683 = ORIENTED_EDGE ( 'NONE', *, *, #10415, .F. ) ;
#14684 = VERTEX_POINT ( 'NONE', #12610 ) ;
#14685 = CARTESIAN_POINT ( 'NONE',  ( 26.03917326857634151, -4.899642733102906433, 7.939653947423662039 ) ) ;
#14686 = CARTESIAN_POINT ( 'NONE',  ( 32.19919549706052209, -6.038393303862174655, 6.861505862736157368 ) ) ;
#14687 = ORIENTED_EDGE ( 'NONE', *, *, #7811, .T. ) ;
#14688 = CARTESIAN_POINT ( 'NONE',  ( 23.47400307746859482, -29.47066586337335892, -14.90105725137469506 ) ) ;
#14689 = CARTESIAN_POINT ( 'NONE',  ( 29.79859849048667897, -1.928627242885762705, -5.783357778048664244 ) ) ;
#14690 = DIRECTION ( 'NONE',  ( 0.000000000000000000, 1.000000000000000000, -0.000000000000000000 ) ) ;
#14691 = CARTESIAN_POINT ( 'NONE',  ( 28.08810621022444920, -4.652786776866828511, -3.627061608673664672 ) ) ;
#14692 = CARTESIAN_POINT ( 'NONE',  ( -23.00000000000000000, -16.21813761408365195, -13.00000000000000178 ) ) ;
#14693 = LINE ( 'NONE', #2275, #6098 ) ;
#14694 = FACE_OUTER_BOUND ( 'NONE', #12894, .T. ) ;
#14695 = FACE_OUTER_BOUND ( 'NONE', #4641, .T. ) ;
#14696 = CARTESIAN_POINT ( 'NONE',  ( 1.296864337298335788E-21, -1.182044466681725685E-21, -6.899999999999998579 ) ) ;
#14697 =( NAMED_UNIT ( * ) SI_UNIT ( $, .STERADIAN. ) SOLID_ANGLE_UNIT ( ) );
#14698 = ADVANCED_FACE ( 'NONE', ( #189 ), #4555, .T. ) ;
#14699 = CARTESIAN_POINT ( 'NONE',  ( 32.17274868998081416, -2.279756424927169345, -4.705209693361160461 ) ) ;
#14700 = CARTESIAN_POINT ( 'NONE',  ( 30.91186687973582536, -2.431667782610909434, -4.705209693361160461 ) ) ;
#14701 = VERTEX_POINT ( 'NONE', #15326 ) ;
#14702 = ORIENTED_EDGE ( 'NONE', *, *, #2806, .F. ) ;
#14703 = CARTESIAN_POINT ( 'NONE',  ( 25.95846283556874212, -3.455553161483297053, 3.283357778048666464 ) ) ;
#14704 = DIRECTION ( 'NONE',  ( 0.9928203230275512992, 0.1196152422706610735, 9.614813431917828943E-17 ) ) ;
#14705 = AXIS2_PLACEMENT_3D ( 'NONE', #13278, #858, #8010 ) ;
#14706 = ORIENTED_EDGE ( 'NONE', *, *, #837, .F. ) ;
#14707 = CARTESIAN_POINT ( 'NONE',  ( 33.20550441965735899, -6.554320347036139971, -5.113484796970860558 ) ) ;
#14708 = EDGE_CURVE ( 'NONE', #3354, #3428, #4357, .T. ) ;
#14709 = CARTESIAN_POINT ( 'NONE',  ( 30.67110321781257909, -3.087645581983020637, -7.939653947423660263 ) ) ;
#14710 = ORIENTED_EDGE ( 'NONE', *, *, #15074, .F. ) ;
#14711 = CARTESIAN_POINT ( 'NONE',  ( 29.46348657678868577, -6.667800981652280967, -7.033357778048666908 ) ) ;
#14712 = CARTESIAN_POINT ( 'NONE',  ( 27.92107091181166467, -2.492190854301117753, -4.533357778048659803 ) ) ;
#14713 = CARTESIAN_POINT ( 'NONE',  ( -6.000000000000000888, 0.000000000000000000, -1.901951201008075243 ) ) ;
#14714 = CARTESIAN_POINT ( 'NONE',  ( 26.31556265977298992, -7.384422263489805793, -5.783357778048663356 ) ) ;
#14715 = ORIENTED_EDGE ( 'NONE', *, *, #16237, .F. ) ;
#14716 = CARTESIAN_POINT ( 'NONE',  ( 32.19529564017040002, -1.250324391365404741, -5.783357778048658027 ) ) ;
#14717 = AXIS2_PLACEMENT_3D ( 'NONE', #14433, #13066, #13243 ) ;
#14718 = CARTESIAN_POINT ( 'NONE',  ( 28.12741954877813555, -2.767138697495831856, -6.861505862736159145 ) ) ;
#14719 = CARTESIAN_POINT ( 'NONE',  ( 11.29999999999999893, 1.383850883036509067E-15, 0.000000000000000000 ) ) ;
#14720 = CARTESIAN_POINT ( 'NONE',  ( 5.000000000000004441, 0.000000000000000000, 0.000000000000000000 ) ) ;
#14721 = DIRECTION ( 'NONE',  ( -1.000000000000000000, 0.000000000000000000, 0.000000000000000000 ) ) ;
#14722 = CARTESIAN_POINT ( 'NONE',  ( 27.42949161418789572, -3.278323244185609830, -3.283357778048662023 ) ) ;
#14723 = ADVANCED_FACE ( 'NONE', ( #9688 ), #16517, .T. ) ;
#14724 = CARTESIAN_POINT ( 'NONE',  ( 32.14665875496697822, -6.044722943765660439, -6.861505862736166250 ) ) ;
#14725 = EDGE_LOOP ( 'NONE', ( #16982, #16528, #10880, #16051 ) ) ;
#14726 = EDGE_CURVE ( 'NONE', #6664, #14530, #17914, .T. ) ;
#14727 = VECTOR ( 'NONE', #17657, 1000.000000000000000 ) ;
#14728 = CYLINDRICAL_SURFACE ( 'NONE', #17050, 2.749999999999992006 ) ;
#14729 = CARTESIAN_POINT ( 'NONE',  ( -27.17934203385504333, -30.00000000000000355, -13.93658524716016878 ) ) ;
#14730 = AXIS2_PLACEMENT_3D ( 'NONE', #1292, #13793, #6816 ) ;
#14731 = ORIENTED_EDGE ( 'NONE', *, *, #4285, .T. ) ;
#14732 = DIRECTION ( 'NONE',  ( -0.9928203230275512992, -0.1196152422706610180, -4.006172263299093133E-17 ) ) ;
#14733 = PLANE ( 'NONE',  #2939 ) ;
#14734 = CARTESIAN_POINT ( 'NONE',  ( 1.296864337298335788E-21, -1.182044466681725685E-21, -6.899999999999998579 ) ) ;
#14735 = CARTESIAN_POINT ( 'NONE',  ( 32.87199790123699472, -1.558343308739095656, 5.783357778048663356 ) ) ;
#14736 = CARTESIAN_POINT ( 'NONE',  ( 27.41826274939272423, -4.733489685532582314, -8.283357778048662468 ) ) ;
#14737 = CARTESIAN_POINT ( 'NONE',  ( 26.18940075748478691, -6.337263906362392341, 3.743184633113769699 ) ) ;
#14738 = DIRECTION ( 'NONE',  ( 0.000000000000000000, 3.469446951953614189E-16, 1.000000000000000000 ) ) ;
#14739 = DIRECTION ( 'NONE',  ( 0.9928203230275510771, 0.1196152422706609902, 4.006172263299092517E-17 ) ) ;
#14740 = EDGE_LOOP ( 'NONE', ( #17431, #7720, #10067, #10164, #17933 ) ) ;
#14741 = CARTESIAN_POINT ( 'NONE',  ( 30.80679339554874119, -2.444327062417882779, -6.861505862736158257 ) ) ;
#14742 = CIRCLE ( 'NONE', #2009, 11.80000000000000249 ) ;
#14743 = DIRECTION ( 'NONE',  ( -0.1196152422706606572, 0.9928203230275512992, 0.000000000000000000 ) ) ;
#14744 = CARTESIAN_POINT ( 'NONE',  ( 33.23365877489121090, -6.550928303235100891, -5.783357778048663356 ) ) ;
#14745 = CARTESIAN_POINT ( 'NONE',  ( 25.93488947238681774, -5.606027099510431988, 3.627061608673663784 ) ) ;
#14746 = ORIENTED_EDGE ( 'NONE', *, *, #8118, .T. ) ;
#14747 = VERTEX_POINT ( 'NONE', #6897 ) ;
#14748 = ADVANCED_FACE ( 'NONE', ( #17905 ), #8178, .F. ) ;
#14749 = CARTESIAN_POINT ( 'NONE',  ( 29.66420847303068697, -4.462897579762144851, 3.627061608673664228 ) ) ;
#14750 = CARTESIAN_POINT ( 'NONE',  ( 32.22908376348204484, -1.973160382215000785, -7.033357778048658027 ) ) ;
#14751 = ORIENTED_EDGE ( 'NONE', *, *, #5656, .T. ) ;
#14752 = CARTESIAN_POINT ( 'NONE',  ( 32.87199790123699472, -1.558343308739095656, -5.783357778048663356 ) ) ;
#14753 = CIRCLE ( 'NONE', #6344, 3.425051884552432035 ) ;
#14754 = CARTESIAN_POINT ( 'NONE',  ( 20.00000000000000000, 7.999999999999996447, 6.000000000000000000 ) ) ;
#14755 = ADVANCED_FACE ( 'NONE', ( #1648 ), #5612, .T. ) ;
#14756 = ORIENTED_EDGE ( 'NONE', *, *, #15699, .T. ) ;
#14757 = ORIENTED_EDGE ( 'NONE', *, *, #16135, .T. ) ;
#14758 = CARTESIAN_POINT ( 'NONE',  ( -45.50000000000000000, -19.03270077640483038, -2.787981825772258837 ) ) ;
#14759 = CARTESIAN_POINT ( 'NONE',  ( 31.87075164095941915, -4.197052703815608687, -3.627061608673664672 ) ) ;
#14760 = CARTESIAN_POINT ( 'NONE',  ( 31.25770402584614516, -1.763030703431812674, -5.783357778048658027 ) ) ;
#14761 = DIRECTION ( 'NONE',  ( -0.9928203230275510771, -0.1196152422706614760, -0.000000000000000000 ) ) ;
#14762 = CARTESIAN_POINT ( 'NONE',  ( 31.71123609653335507, -2.762457591843783256, -8.283357778048660691 ) ) ;
#14763 = CARTESIAN_POINT ( 'NONE',  ( 30.06013935859953534, -5.869009311960809328, -8.283357778048664244 ) ) ;
#14764 = AXIS2_PLACEMENT_3D ( 'NONE', #10094, #17397, #2053 ) ;
#14765 =( BOUNDED_CURVE ( )  B_SPLINE_CURVE ( 2, ( #10464, #13197, #6119, #11647, #15745, #3225, #10367, #15829, #8668 ),
 .UNSPECIFIED., .F., .T. ) 
 B_SPLINE_CURVE_WITH_KNOTS ( ( 3, 2, 2, 2, 3 ),
 ( 0.2884615384615384914, 0.2948717948717948789, 0.3076923076923077094, 0.3205128205128205399, 0.3269230769230769273 ),
 .UNSPECIFIED. ) 
 CURVE ( )  GEOMETRIC_REPRESENTATION_ITEM ( )  RATIONAL_B_SPLINE_CURVE ( ( 0.9330127018922194093, 0.9330127018922196314, 1.000000000000000000, 0.8660254037844387076, 1.000000000000000000, 0.8660254037844387076, 1.000000000000000000, 0.9330127018922194093, 0.9330127018922194093 ) ) 
 REPRESENTATION_ITEM ( '' )  );
#14766 = CARTESIAN_POINT ( 'NONE',  ( 29.37220822929407760, -7.016156836349003001, -5.783357778048668685 ) ) ;
#14767 = CARTESIAN_POINT ( 'NONE',  ( 32.29295089585318834, -5.599999616269981217, -3.283357778048667797 ) ) ;
#14768 = CARTESIAN_POINT ( 'NONE',  ( 29.84999239022537409, -5.894327871574777333, 8.283357778048658915 ) ) ;
#14769 = ORIENTED_EDGE ( 'NONE', *, *, #15671, .F. ) ;
#14770 = ORIENTED_EDGE ( 'NONE', *, *, #1268, .T. ) ;
#14771 = CARTESIAN_POINT ( 'NONE',  ( 31.71314141467879111, -4.216041623526076698, 7.939653947423662039 ) ) ;
#14772 = VECTOR ( 'NONE', #14038, 1000.000000000000000 ) ;
#14773 = CARTESIAN_POINT ( 'NONE',  ( 29.65098506949083301, -2.583579140294649523, 6.861505862736166250 ) ) ;
#14774 = EDGE_LOOP ( 'NONE', ( #3606, #3256, #7740, #715, #5636 ) ) ;
#14775 = DIRECTION ( 'NONE',  ( -0.000000000000000000, -0.000000000000000000, -1.000000000000000000 ) ) ;
#14776 = LINE ( 'NONE', #11857, #2884 ) ;
#14777 = ADVANCED_FACE ( 'NONE', ( #12692 ), #4187, .T. ) ;
#14778 = DIRECTION ( 'NONE',  ( -0.9237280213470682178, -0.3830490080632377170, 0.000000000000000000 ) ) ;
#14779 = CARTESIAN_POINT ( 'NONE',  ( 29.76058531221316628, -5.705227139567997874, -7.939653947423664704 ) ) ;
#14780 = CARTESIAN_POINT ( 'NONE',  ( -5.499998817156067865, -20.49639288455253450, -13.00000000000000178 ) ) ;
#14781 = AXIS2_PLACEMENT_3D ( 'NONE', #11443, #3213, #1870 ) ;
#14782 = CARTESIAN_POINT ( 'NONE',  ( 31.29094215978502547, -2.813094711071706389, -3.283357778048662023 ) ) ;
#14783 = LINE ( 'NONE', #7531, #13374 ) ;
#14784 = CARTESIAN_POINT ( 'NONE',  ( 26.87859896403794835, -7.316587507915443211, -6.453230759126474148 ) ) ;
#14785 = SURFACE_SIDE_STYLE ('',( #7626 ) ) ;
#14786 = CARTESIAN_POINT ( 'NONE',  ( 32.18597209352066812, -4.159074864394664672, -7.939653947423662039 ) ) ;
#14787 = CARTESIAN_POINT ( 'NONE',  ( 31.55553118839817728, -4.235030543236534939, -7.939653947423662039 ) ) ;
#14788 = ORIENTED_EDGE ( 'NONE', *, *, #4330, .F. ) ;
#14789 = LINE ( 'NONE', #12048, #15283 ) ;
#14790 = DIRECTION ( 'NONE',  ( -0.000000000000000000, -0.000000000000000000, -1.000000000000000000 ) ) ;
#14791 = ORIENTED_EDGE ( 'NONE', *, *, #7563, .T. ) ;
#14792 = CARTESIAN_POINT ( 'NONE',  ( 33.23365877489121090, -6.550928303235100891, -5.783357778048663356 ) ) ;
#14793 = CARTESIAN_POINT ( 'NONE',  ( 30.86385689617753059, -5.572304701594727128, -7.939653947423662927 ) ) ;
#14794 = EDGE_CURVE ( 'NONE', #13014, #17268, #8027, .T. ) ;
#14795 = DIRECTION ( 'NONE',  ( 0.000000000000000000, 0.000000000000000000, 1.000000000000000000 ) ) ;
#14796 = DIRECTION ( 'NONE',  ( 0.000000000000000000, 0.000000000000000000, 1.000000000000000000 ) ) ;
#14797 = EDGE_CURVE ( 'NONE', #16037, #963, #10258, .T. ) ;
#14798 = CARTESIAN_POINT ( 'NONE',  ( 25.92409770820621162, -4.135217962343409326, 7.801241002635260102 ) ) ;
#14799 = LINE ( 'NONE', #13249, #6711 ) ;
#14800 = CARTESIAN_POINT ( 'NONE',  ( 31.03206908560819954, -5.751910973953720863, -3.283357778048667797 ) ) ;
#14801 = AXIS2_PLACEMENT_3D ( 'NONE', #5882, #6983, #1730 ) ;
#14802 = ORIENTED_EDGE ( 'NONE', *, *, #1689, .T. ) ;
#14803 =( GEOMETRIC_REPRESENTATION_CONTEXT ( 3 ) GLOBAL_UNCERTAINTY_ASSIGNED_CONTEXT ( ( #4134 ) ) GLOBAL_UNIT_ASSIGNED_CONTEXT ( ( #12860, #7156, #526 ) ) REPRESENTATION_CONTEXT ( 'NONE', 'WORKASPACE' ) );
#14804 = CARTESIAN_POINT ( 'NONE',  ( 33.17094678975809074, -2.159493266760871499, -6.861505862736159145 ) ) ;
#14805 = CARTESIAN_POINT ( 'NONE',  ( 2.500000000000000000, -1.178949249685213863, 2.042000000000001148 ) ) ;
#14806 = CARTESIAN_POINT ( 'NONE',  ( 1.144235203016664926, 3.958177651039091582, -0.09382832055445673725 ) ) ;
#14807 = DIRECTION ( 'NONE',  ( 1.000000000000000000, 0.000000000000000000, 0.000000000000000000 ) ) ;
#14808 = CARTESIAN_POINT ( 'NONE',  ( 27.18555652250208610, -2.580805812949960920, -7.033357778048658027 ) ) ;
#14809 = CARTESIAN_POINT ( 'NONE',  ( 30.90769699326645181, -6.820963901304073929, -5.783357778048668685 ) ) ;
#14810 = AXIS2_PLACEMENT_3D ( 'NONE', #73, #3309, #5585 ) ;
#14811 = CARTESIAN_POINT ( 'NONE',  ( 23.00000000000000000, -16.21813761408365195, 13.00000000000000355 ) ) ;
#14812 = CARTESIAN_POINT ( 'NONE',  ( 3.349226789952651995, 2.685125164760732819, -0.2236248678334793738 ) ) ;
#14813 = ORIENTED_EDGE ( 'NONE', *, *, #11266, .T. ) ;
#14814 = DIRECTION ( 'NONE',  ( -1.224646799147353207E-16, 1.000000000000000000, 0.000000000000000000 ) ) ;
#14815 = ADVANCED_FACE ( 'NONE', ( #14677, #7775 ), #10145, .T. ) ;
#14816 = CARTESIAN_POINT ( 'NONE',  ( 33.46007730730551799, -5.886481946178435010, -4.705209693361169343 ) ) ;
#14817 = CARTESIAN_POINT ( 'NONE',  ( 30.06013935859953534, -5.869009311960809328, 3.283357778048663356 ) ) ;
#14818 = AXIS2_PLACEMENT_3D ( 'NONE', #11204, #5602, #3083 ) ;
#14819 = CARTESIAN_POINT ( 'NONE',  ( 26.63392073224175505, -2.647267031729148012, -7.033357778048658027 ) ) ;
#14820 = CARTESIAN_POINT ( 'NONE',  ( -21.42601376483257880, 2.765314980223223529, 0.000000000000000000 ) ) ;
#14821 = CARTESIAN_POINT ( 'NONE',  ( 4.211140560182196957, -2.431303136016550237, -3.445885042887436800 ) ) ;
#14822 = CARTESIAN_POINT ( 'NONE',  ( 26.01652455409633902, -4.902371455920926380, -5.783357778048663356 ) ) ;
#14823 = ORIENTED_EDGE ( 'NONE', *, *, #13608, .F. ) ;
#14824 = AXIS2_PLACEMENT_3D ( 'NONE', #16623, #4201, #1303 ) ;
#14825 = CARTESIAN_POINT ( 'NONE',  ( 31.04338717100262102, -6.177645381738930297, -6.861505862736167138 ) ) ;
#14826 = AXIS2_PLACEMENT_3D ( 'NONE', #14734, #17577, #3849 ) ;
#14827 = CARTESIAN_POINT ( 'NONE',  ( 33.27602027394517847, -2.146833986953896822, -4.705209693361161349 ) ) ;
#14828 = CARTESIAN_POINT ( 'NONE',  ( 33.95908713831673964, -3.945449517755641455, 8.283357778048662468 ) ) ;
#14829 = CARTESIAN_POINT ( 'NONE',  ( 31.12210306526553083, -4.287250072544045665, 3.283357778048664244 ) ) ;
#14830 = ORIENTED_EDGE ( 'NONE', *, *, #10359, .F. ) ;
#14831 = VECTOR ( 'NONE', #11903, 1000.000000000000000 ) ;
#14832 = ORIENTED_EDGE ( 'NONE', *, *, #532, .F. ) ;
#14833 = CARTESIAN_POINT ( 'NONE',  ( 29.55043834383899437, -5.730545699181964991, 7.939653947423658487 ) ) ;
#14834 = CARTESIAN_POINT ( 'NONE',  ( 16.79145860028663151, -17.04903085677362640, 16.02982020200856184 ) ) ;
#14835 = ORIENTED_EDGE ( 'NONE', *, *, #12230, .T. ) ;
#14836 = DIRECTION ( 'NONE',  ( 0.9928203230275510771, 0.1196152422706614205, 0.000000000000000000 ) ) ;
#14837 = CIRCLE ( 'NONE', #3841, 11.80000000000000249 ) ;
#14838 = EDGE_CURVE ( 'NONE', #7363, #10674, #15350, .T. ) ;
#14839 = VERTEX_POINT ( 'NONE', #17422 ) ;
#14840 = B_SPLINE_CURVE_WITH_KNOTS ( 'NONE', 3,
 ( #13100, #3665, #6482, #10619 ),
 .UNSPECIFIED., .F., .F.,
 ( 4, 4 ),
 ( 2.843119637679310382E-07, 0.001422633878257846627 ),
 .UNSPECIFIED. ) ;
#14841 = DIRECTION ( 'NONE',  ( 1.000000000000000000, 0.000000000000000000, 0.000000000000000000 ) ) ;
#14842 = CARTESIAN_POINT ( 'NONE',  ( 29.77797860222238313, -3.195249460342344250, -3.627061608673662008 ) ) ;
#14843 = VECTOR ( 'NONE', #17952, 1000.000000000000227 ) ;
#14844 = CARTESIAN_POINT ( 'NONE',  ( 30.98067518586950442, -1.786210345264705790, -5.783357778048658027 ) ) ;
#14845 = EDGE_CURVE ( 'NONE', #15676, #947, #14082, .T. ) ;
#14846 = CARTESIAN_POINT ( 'NONE',  ( -20.00000000000000000, 7.999999999999996447, -12.00000000000000000 ) ) ;
#14847 = FACE_OUTER_BOUND ( 'NONE', #3625, .T. ) ;
#14848 = CARTESIAN_POINT ( 'NONE',  ( 26.39379627684682106, -4.856917663858078882, -3.283357778048664688 ) ) ;
#14849 = CARTESIAN_POINT ( 'NONE',  ( 27.53837573810956130, -6.172832027328289506, 3.283357778048663800 ) ) ;
#14850 = EDGE_LOOP ( 'NONE', ( #5890, #3904, #9970, #23, #11322, #10829 ) ) ;
#14851 = EDGE_LOOP ( 'NONE', ( #12103, #12116, #15677, #3905 ) ) ;
#14852 = ORIENTED_EDGE ( 'NONE', *, *, #1084, .T. ) ;
#14853 = ORIENTED_EDGE ( 'NONE', *, *, #7444, .F. ) ;
#14854 = CARTESIAN_POINT ( 'NONE',  ( 31.27962407439061110, -2.387360303286481855, 4.705209693361167567 ) ) ;
#14855 = CARTESIAN_POINT ( 'NONE',  ( 30.91186687973582536, -2.431667782610909434, 6.861505862736166250 ) ) ;
#14856 = ORIENTED_EDGE ( 'NONE', *, *, #9266, .T. ) ;
#14857 = FACE_OUTER_BOUND ( 'NONE', #8450, .T. ) ;
#14858 = CARTESIAN_POINT ( 'NONE',  ( 3.000000000000000000, 0.000000000000000000, 1.599999999999998979 ) ) ;
#14859 = FACE_BOUND ( 'NONE', #13882, .T. ) ;
#14860 = CARTESIAN_POINT ( 'NONE',  ( 30.43486631442457835, -6.877930660435475296, -5.783357778048669573 ) ) ;
#14861 = DIRECTION ( 'NONE',  ( 0.000000000000000000, 0.000000000000000000, 1.000000000000000000 ) ) ;
#14862 = ORIENTED_EDGE ( 'NONE', *, *, #7981, .T. ) ;
#14863 = CARTESIAN_POINT ( 'NONE',  ( 33.27992013083530054, -6.934902899450660740, -5.783357778048669573 ) ) ;
#14864 = CARTESIAN_POINT ( 'NONE',  ( 31.68992120585416217, -1.700760206360153015, 5.783357778048662468 ) ) ;
#14865 = CARTESIAN_POINT ( 'NONE',  ( 27.25621498173240198, -3.499072175709823984, -3.627061608673662008 ) ) ;
#14866 = CARTESIAN_POINT ( 'NONE',  ( 18.90607966454165734, -11.47788193099826692, 15.70134094032044736 ) ) ;
#14867 = ORIENTED_EDGE ( 'NONE', *, *, #4107, .T. ) ;
#14868 = CARTESIAN_POINT ( 'NONE',  ( 30.39102621733566423, -5.629271460726126719, -7.939653947423664704 ) ) ;
#14869 = VECTOR ( 'NONE', #14395, 1000.000000000000000 ) ;
#14870 = VERTEX_POINT ( 'NONE', #6417 ) ;
#14871 = DIRECTION ( 'NONE',  ( 5.026720092345836698E-22, -4.581671729415424240E-22, 1.000000000000000000 ) ) ;
#14872 = AXIS2_PLACEMENT_3D ( 'NONE', #10139, #10313, #1478 ) ;
#14873 = ADVANCED_FACE ( 'NONE', ( #12786 ), #3616, .T. ) ;
#14874 = LINE ( 'NONE', #2461, #909 ) ;
#14875 = B_SPLINE_CURVE_WITH_KNOTS ( 'NONE', 3,
 ( #4681, #8863, #14033, #14394, #4506, #10019 ),
 .UNSPECIFIED., .F., .F.,
 ( 4, 2, 4 ),
 ( -3.640115492407988208E-06, 0.0002066546034006553050, 0.0004169493222937186317 ),
 .UNSPECIFIED. ) ;
#14876 = ORIENTED_EDGE ( 'NONE', *, *, #16280, .F. ) ;
#14877 = CARTESIAN_POINT ( 'NONE',  ( 31.25770402584614871, -1.763030703431812451, 5.783357778048668685 ) ) ;
#14878 = CARTESIAN_POINT ( 'NONE',  ( 30.15026255541241440, -6.285249260098253465, -4.705209693361168455 ) ) ;
#14879 = EDGE_CURVE ( 'NONE', #4281, #14662, #5974, .T. ) ;
#14880 = LINE ( 'NONE', #6619, #5530 ) ;
#14881 = CARTESIAN_POINT ( 'NONE',  ( 33.95908713831674675, -3.945449517755636126, -5.783357778048663356 ) ) ;
#14882 = CARTESIAN_POINT ( 'NONE',  ( 28.58911057998038885, -6.046239229258517867, -3.283357778048667797 ) ) ;
#14883 = CYLINDRICAL_SURFACE ( 'NONE', #925, 12.50000000000000000 ) ;
#14884 = CARTESIAN_POINT ( 'NONE',  ( 32.57067411085063924, -7.020353038355215070, -5.783357778048669573 ) ) ;
#14885 = ORIENTED_EDGE ( 'NONE', *, *, #16722, .T. ) ;
#14886 = CARTESIAN_POINT ( 'NONE',  ( 33.42946061375642586, -6.517141185936593750, -5.783357778048668685 ) ) ;
#14887 = CARTESIAN_POINT ( 'NONE',  ( 26.30054492745253825, -7.259773351106304951, -5.235134217867734030 ) ) ;
#14888 = CARTESIAN_POINT ( 'NONE',  ( 30.35023428074701002, -1.862166024106576057, -5.783357778048664244 ) ) ;
#14889 = CARTESIAN_POINT ( 'NONE',  ( 1.287221018261662353, 3.875624752116917371, -3.130620751972434501 ) ) ;
#14890 = CARTESIAN_POINT ( 'NONE',  ( 26.14503574297738098, -5.691300421908874085, -8.283357778048664244 ) ) ;
#14891 = EDGE_CURVE ( 'NONE', #9479, #5360, #7605, .T. ) ;
#14892 = CARTESIAN_POINT ( 'NONE',  ( 32.51858583609114106, -1.611119345748072362, -5.783357778048658915 ) ) ;
#14893 = EDGE_CURVE ( 'NONE', #7696, #6789, #7159, .T. ) ;
#14894 = ORIENTED_EDGE ( 'NONE', *, *, #16135, .F. ) ;
#14895 = AXIS2_PLACEMENT_3D ( 'NONE', #1686, #16736, #11542 ) ;
#14896 = ORIENTED_EDGE ( 'NONE', *, *, #6742, .T. ) ;
#14897 = DIRECTION ( 'NONE',  ( 0.000000000000000000, 0.000000000000000000, -1.000000000000000000 ) ) ;
#14898 = CARTESIAN_POINT ( 'NONE',  ( -27.54501800341186168, -11.92321325334030568, -13.84074570522889047 ) ) ;
#14899 = ORIENTED_EDGE ( 'NONE', *, *, #12945, .T. ) ;
#14900 = FACE_OUTER_BOUND ( 'NONE', #15748, .T. ) ;
#14901 = CARTESIAN_POINT ( 'NONE',  ( 33.32855701603872234, -2.140504347050403045, -6.861505862736158257 ) ) ;
#14902 = CARTESIAN_POINT ( 'NONE',  ( 4.154306624730766728, 2.398490048085576642, -3.421999068284416357 ) ) ;
#14903 = CARTESIAN_POINT ( 'NONE',  ( 26.94172295629870462, -6.971623697019761146, -7.033357778048666908 ) ) ;
#14904 = CARTESIAN_POINT ( 'NONE',  ( -8.250000000000060396, -6.495190528383215423, -3.000000000000000000 ) ) ;
#14905 = CARTESIAN_POINT ( 'NONE',  ( 25.71748644841968456, -2.420320648352046078, -5.783357778048663356 ) ) ;
#14906 = CARTESIAN_POINT ( 'NONE',  ( 25.76326615456878244, -3.051972493152843580, -6.861505862736158257 ) ) ;
#14907 = ADVANCED_FACE ( 'NONE', ( #12967 ), #8715, .T. ) ;
#14908 = CARTESIAN_POINT ( 'NONE',  ( 29.03578327489625011, -17.85349083735938081, -13.43326801114178615 ) ) ;
#14909 = CARTESIAN_POINT ( 'NONE',  ( 31.07327543742414022, -2.112412460091767308, 7.033357778048666020 ) ) ;
#14910 = ORIENTED_EDGE ( 'NONE', *, *, #6235, .T. ) ;
#14911 = EDGE_CURVE ( 'NONE', #10340, #122, #159, .T. ) ;
#14912 = ORIENTED_EDGE ( 'NONE', *, *, #11306, .T. ) ;
#14913 = CARTESIAN_POINT ( 'NONE',  ( 28.28502977505876359, -2.748149777785362957, 4.705209693361168455 ) ) ;
#14914 = CARTESIAN_POINT ( 'NONE',  ( -20.00000000000000000, 7.999999999999996447, 0.000000000000000000 ) ) ;
#14915 = CARTESIAN_POINT ( 'NONE',  ( 22.22189723075623036, -22.43265299876153662, 15.08700452545048343 ) ) ;
#14916 = EDGE_CURVE ( 'NONE', #10596, #12847, #16131, .T. ) ;
#14917 = EDGE_LOOP ( 'NONE', ( #10108, #669, #2415, #15715 ) ) ;
#14918 = CARTESIAN_POINT ( 'NONE',  ( 27.17934203385504333, -30.00000000000000355, 12.00000000000000000 ) ) ;
#14919 = EDGE_LOOP ( 'NONE', ( #12432, #15850, #9168, #708 ) ) ;
#14920 = EDGE_LOOP ( 'NONE', ( #14325, #12741, #4851 ) ) ;
#14921 = CARTESIAN_POINT ( 'NONE',  ( 46.86575133767495061, -2.390451368237048069, -5.783357778048661579 ) ) ;
#14922 = ORIENTED_EDGE ( 'NONE', *, *, #14845, .F. ) ;
#14923 = DIRECTION ( 'NONE',  ( -0.000000000000000000, -0.000000000000000000, 1.000000000000000000 ) ) ;
#14924 = CARTESIAN_POINT ( 'NONE',  ( 29.78250536075762867, -6.329556739422670830, -6.861505862736167138 ) ) ;
#14925 = PRESENTATION_LAYER_ASSIGNMENT (  '', '', ( #3928 ) ) ;
#14926 = CARTESIAN_POINT ( 'NONE',  ( 30.57046727500519978, -4.353711291323232757, -8.283357778048662468 ) ) ;
#14927 = DIRECTION ( 'NONE',  ( 1.224646799147353207E-16, -1.000000000000000000, 0.000000000000000000 ) ) ;
#14928 = DIRECTION ( 'NONE',  ( -0.9237280213470682178, -0.3830490080632377725, 0.000000000000000000 ) ) ;
#14929 = CARTESIAN_POINT ( 'NONE',  ( 26.03917326857634151, -4.899642733102906433, 7.939653947423662039 ) ) ;
#14930 = ORIENTED_EDGE ( 'NONE', *, *, #3168, .F. ) ;
#14931 = CARTESIAN_POINT ( 'NONE',  ( 27.47505859511117521, -2.218764776483033163, 5.783357778048668685 ) ) ;
#14932 = CARTESIAN_POINT ( 'NONE',  ( 33.66004903264009585, -1.463398710186758267, 5.783357778048663356 ) ) ;
#14933 = CARTESIAN_POINT ( 'NONE',  ( 32.29974222271236073, -2.891426744974864071, 7.939653947423664704 ) ) ;
#14934 = CARTESIAN_POINT ( 'NONE',  ( 29.62480591732145996, -4.467644809586046151, 8.283357778048662468 ) ) ;
#14935 = EDGE_CURVE ( 'NONE', #10223, #15284, #10828, .T. ) ;
#14936 = ORIENTED_EDGE ( 'NONE', *, *, #11713, .T. ) ;
#14937 = ORIENTED_EDGE ( 'NONE', *, *, #11055, .T. ) ;
#14938 = CARTESIAN_POINT ( 'NONE',  ( 30.25080928106424594, -3.138282701210941994, 7.939653947423664704 ) ) ;
#14939 = DIRECTION ( 'NONE',  ( -0.1196152422706598106, 0.9928203230275514102, 0.000000000000000000 ) ) ;
#14940 = EDGE_CURVE ( 'NONE', #7031, #12145, #8615, .T. ) ;
#14941 = CARTESIAN_POINT ( 'NONE',  ( 29.66420847303068697, -4.462897579762144851, 3.627061608673664228 ) ) ;
#14942 = ADVANCED_FACE ( 'NONE', ( #13571 ), #17944, .F. ) ;
#14943 = LINE ( 'NONE', #8309, #11527 ) ;
#14944 = FACE_OUTER_BOUND ( 'NONE', #5012, .T. ) ;
#14945 = CARTESIAN_POINT ( 'NONE',  ( 29.71979337562451207, -1.938121702948446323, -5.783357778048664244 ) ) ;
#14946 = CARTESIAN_POINT ( 'NONE',  ( 29.15206445563513071, -6.405512418264540209, -6.861505862736167138 ) ) ;
#14947 = DIRECTION ( 'NONE',  ( 0.7999999999999999334, -0.6000000000000001998, 0.000000000000000000 ) ) ;
#14948 = CARTESIAN_POINT ( 'NONE',  ( 32.34167700165585302, -2.686501913001913433, -8.283357778048658915 ) ) ;
#14949 = CYLINDRICAL_SURFACE ( 'NONE', #17771, 2.500000000000001776 ) ;
#14950 = CARTESIAN_POINT ( 'NONE',  ( 28.68570264635560463, -13.61469575198669624, -13.53129406029897730 ) ) ;
#14951 = DIRECTION ( 'NONE',  ( 0.9928203230275512992, 0.1196152422706610180, 4.006172263299093133E-17 ) ) ;
#14952 = CARTESIAN_POINT ( 'NONE',  ( 31.67382807612511542, -6.101689702897060030, -6.861505862736167138 ) ) ;
#14953 = CARTESIAN_POINT ( 'NONE',  ( 27.91310269393460430, -7.181753375802955475, -5.783357778048669573 ) ) ;
#14954 = DIRECTION ( 'NONE',  ( -1.000000000000000000, 2.131628207280300558E-14, 0.000000000000000000 ) ) ;
#14955 = EDGE_CURVE ( 'NONE', #6877, #1158, #3840, .T. ) ;
#14956 = DIRECTION ( 'NONE',  ( -1.000000000000000000, 0.000000000000000000, 0.000000000000000000 ) ) ;
#14957 = ORIENTED_EDGE ( 'NONE', *, *, #10328, .T. ) ;
#14958 = CARTESIAN_POINT ( 'NONE',  ( 30.90769699326645181, -6.820963901304073929, 5.783357778048658915 ) ) ;
#14959 = CARTESIAN_POINT ( 'NONE',  ( 28.73594040535617467, -2.066853418799292630, -5.783357778048658915 ) ) ;
#14960 = DIRECTION ( 'NONE',  ( -1.000000000000000000, 0.000000000000000000, 0.000000000000000000 ) ) ;
#14961 = DIRECTION ( 'NONE',  ( 0.000000000000000000, -0.5000000000000009992, -0.8660254037844380415 ) ) ;
#14962 = CARTESIAN_POINT ( 'NONE',  ( 28.76992167940542799, -7.088720471389836852, -6.453230759126468818 ) ) ;
#14963 = CARTESIAN_POINT ( 'NONE',  ( 25.75741033704265703, -2.751693534003877062, 5.593203463216974036 ) ) ;
#14964 = PLANE ( 'NONE',  #4679 ) ;
#14965 = EDGE_CURVE ( 'NONE', #11575, #16655, #5215, .T. ) ;
#14966 = CARTESIAN_POINT ( 'NONE',  ( 33.16732689266149237, -6.221561368663743430, -7.033357778048666908 ) ) ;
#14967 = VERTEX_POINT ( 'NONE', #6674 ) ;
#14968 = CARTESIAN_POINT ( 'NONE',  ( 31.91006497951310550, -2.311404624444611589, -6.861505862736159145 ) ) ;
#14969 = CARTESIAN_POINT ( 'NONE',  ( 26.31376129264122810, -7.369470708288995198, -5.989870097397514748 ) ) ;
#14970 = LINE ( 'NONE', #3736, #12936 ) ;
#14971 = DIRECTION ( 'NONE',  ( -1.000000000000000000, 0.000000000000000000, 0.000000000000000000 ) ) ;
#14972 = DIRECTION ( 'NONE',  ( 0.000000000000000000, -1.000000000000000000, 0.000000000000000000 ) ) ;
#14973 = AXIS2_PLACEMENT_3D ( 'NONE', #12003, #14653, #1043 ) ;
#14974 = ADVANCED_FACE ( 'NONE', ( #10906 ), #17692, .F. ) ;
#14975 = CARTESIAN_POINT ( 'NONE',  ( 32.01513846370018967, -2.298745344637636912, -4.705209693361161349 ) ) ;
#14976 = VERTEX_POINT ( 'NONE', #2691 ) ;
#14977 = AXIS2_PLACEMENT_3D ( 'NONE', #9868, #15423, #14063 ) ;
#14978 = CARTESIAN_POINT ( 'NONE',  ( -11.38175538881593774, -22.33742387525457573, 16.67884400577319681 ) ) ;
#14979 = CARTESIAN_POINT ( 'NONE',  ( 13.00000000000000178, 0.000000000000000000, -8.700000000000001066 ) ) ;
#14980 = VERTEX_POINT ( 'NONE', #14932 ) ;
#14981 = AXIS2_PLACEMENT_3D ( 'NONE', #17533, #15955, #2090 ) ;
#14982 = CARTESIAN_POINT ( 'NONE',  ( 29.97942892559193950, -4.424919740341219487, -3.627061608673664672 ) ) ;
#14983 = ADVANCED_FACE ( 'NONE', ( #5388 ), #16557, .T. ) ;
#14984 = CARTESIAN_POINT ( 'NONE',  ( 2.500000000000000000, 1.178949249685213863, -2.042000000000001148 ) ) ;
#14985 = VERTEX_POINT ( 'NONE', #12471 ) ;
#14986 = CARTESIAN_POINT ( 'NONE',  ( 32.65880277236253448, -4.102108105263264193, -7.939653947423662039 ) ) ;
#14987 = LINE ( 'NONE', #16452, #15615 ) ;
#14988 = CARTESIAN_POINT ( 'NONE',  ( 3.999999999999998224, 0.000000000000000000, 0.000000000000000000 ) ) ;
#14989 = CARTESIAN_POINT ( 'NONE',  ( 33.64386668575551198, -3.983427357176565486, -8.283357778048662468 ) ) ;
#14990 = CARTESIAN_POINT ( 'NONE',  ( 25.90899358965569022, -2.397247819800704782, -6.453230759126464378 ) ) ;
#14991 = CARTESIAN_POINT ( 'NONE',  ( 32.29295089585319545, -5.599999616269980329, 8.283357778048658915 ) ) ;
#14992 = PRODUCT_DEFINITION ( 'UNKNOWN', '', #8028, #5382 ) ;
#14993 = CIRCLE ( 'NONE', #12104, 5.000000000000000888 ) ;
#14994 = CARTESIAN_POINT ( 'NONE',  ( 28.52162355051263987, -6.481468097106410475, 4.705209693361159573 ) ) ;
#14995 = CARTESIAN_POINT ( 'NONE',  ( -4.198928548860774157, 0.8158838809860086139, -3.226471437616920124 ) ) ;
#14996 = ORIENTED_EDGE ( 'NONE', *, *, #15533, .T. ) ;
#14997 = DIRECTION ( 'NONE',  ( 0.9928203230275510771, 0.1196152422706609902, 4.006172263299092517E-17 ) ) ;
#14998 = CIRCLE ( 'NONE', #17362, 10.50000000000000000 ) ;
#14999 = ORIENTED_EDGE ( 'NONE', *, *, #2122, .F. ) ;
#15000 = CARTESIAN_POINT ( 'NONE',  ( 9.099998387031005720, -19.29508120620799971, 16.81964500401478091 ) ) ;
#15001 = ADVANCED_FACE ( 'NONE', ( #9389 ), #8218, .F. ) ;
#15002 = VERTEX_POINT ( 'NONE', #6937 ) ;
#15003 = CYLINDRICAL_SURFACE ( 'NONE', #13402, 6.000000000000000888 ) ;
#15004 = EDGE_CURVE ( 'NONE', #16224, #2940, #2963, .T. ) ;
#15005 = CARTESIAN_POINT ( 'NONE',  ( 28.39010325924584421, -2.735490497978389612, -4.705209693361160461 ) ) ;
#15006 = CARTESIAN_POINT ( 'NONE',  ( 30.72436838703367812, -6.515889623968540434, -7.033357778048666908 ) ) ;
#15007 = CARTESIAN_POINT ( 'NONE',  ( 26.85044460880409645, -7.319979551716484067, 5.783357778048657138 ) ) ;
#15008 = CARTESIAN_POINT ( 'NONE',  ( 0.000000000000000000, 0.000000000000000000, 11.56671555609732671 ) ) ;
#15009 = CARTESIAN_POINT ( 'NONE',  ( 25.71072941247523502, -3.058302133056337357, 6.861505862736165362 ) ) ;
#15010 = CARTESIAN_POINT ( 'NONE',  ( 29.19137779418881351, -4.519864338893556877, 7.939653947423662039 ) ) ;
#15011 = DIRECTION ( 'NONE',  ( 0.9928203230275512992, 0.1196152422706610180, 4.006172263299093133E-17 ) ) ;
#15012 = CARTESIAN_POINT ( 'NONE',  ( 27.30498922523054617, -2.229057914452205136, -5.113484796970851676 ) ) ;
#15013 = CARTESIAN_POINT ( 'NONE',  ( 32.72003615946069743, -2.840789625746940938, 3.627061608673666893 ) ) ;
#15014 = EDGE_LOOP ( 'NONE', ( #3500, #12948 ) ) ;
#15015 = CARTESIAN_POINT ( 'NONE',  ( 28.20260476654369697, -6.819712339336020612, 4.533357778048659803 ) ) ;
#15016 = VERTEX_POINT ( 'NONE', #6768 ) ;
#15017 = ORIENTED_EDGE ( 'NONE', *, *, #13123, .T. ) ;
#15018 = VECTOR ( 'NONE', #14369, 1000.000000000000000 ) ;
#15019 = ORIENTED_EDGE ( 'NONE', *, *, #2382, .F. ) ;
#15020 = CARTESIAN_POINT ( 'NONE',  ( 32.54503264317084188, -5.369756224683081669, 7.939653947423658487 ) ) ;
#15021 = CARTESIAN_POINT ( 'NONE',  ( 28.55903157092087952, -3.142235986053133256, -8.283357778048660691 ) ) ;
#15022 = VERTEX_POINT ( 'NONE', #4142 ) ;
#15023 = CARTESIAN_POINT ( 'NONE',  ( 29.78250536075762867, -6.329556739422670830, 4.705209693361159573 ) ) ;
#15024 = EDGE_LOOP ( 'NONE', ( #14220, #429 ) ) ;
#15025 = CARTESIAN_POINT ( 'NONE',  ( 31.29168529989541270, -6.784897756022354010, -6.453230759126470595 ) ) ;
#15026 = CYLINDRICAL_SURFACE ( 'NONE', #16222, 12.50000000000000000 ) ;
#15027 = CYLINDRICAL_SURFACE ( 'NONE', #15394, 2.500000000000001776 ) ;
#15028 = CARTESIAN_POINT ( 'NONE',  ( 27.00222791626931595, -2.275731535614434531, -5.783357778048658027 ) ) ;
#15029 = CARTESIAN_POINT ( 'NONE',  ( 30.54048978798443059, -6.538043363838207611, 7.033357778048657138 ) ) ;
#15030 = VECTOR ( 'NONE', #4309, 1000.000000000000000 ) ;
#15032 = EDGE_CURVE ( 'NONE', #10872, #5499, #16564, .T. ) ;
#15031 = CARTESIAN_POINT ( 'NONE',  ( 27.99987602667382802, -2.482696394238434578, -4.533357778048659803 ) ) ;
#15033 = CARTESIAN_POINT ( 'NONE',  ( -3.199999999999998845, 3.918869757271528981E-16, 1.599999999999999423 ) ) ;
#15034 = CARTESIAN_POINT ( 'NONE',  ( 20.84129949943806537, -10.34926000617958231, -15.35708546568073984 ) ) ;
#15035 = CARTESIAN_POINT ( 'NONE',  ( 26.47260139170898441, -4.847423203795396596, 8.283357778048662468 ) ) ;
#15036 = TOROIDAL_SURFACE ( 'NONE', #1438, 12.70000000000000284, 0.9000000000000003553 ) ;
#15037 = CARTESIAN_POINT ( 'NONE',  ( 30.15443244188179150, -1.895953141405084086, -5.783357778048658027 ) ) ;
#15038 = EDGE_CURVE ( 'NONE', #11629, #8286, #15195, .T. ) ;
#15039 = CARTESIAN_POINT ( 'NONE',  ( 29.80442540930208750, -6.953886339277345563, -5.783357778048669573 ) ) ;
#15040 = VERTEX_POINT ( 'NONE', #3957 ) ;
#15041 = CARTESIAN_POINT ( 'NONE',  ( 0.000000000000000000, 0.000000000000000000, -4.674599999999997202 ) ) ;
#15042 = CARTESIAN_POINT ( 'NONE',  ( -7.499998387031003411, -20.49508120620799900, 13.00000000000000178 ) ) ;
#15043 = CIRCLE ( 'NONE', #2028, 2.500000000000000888 ) ;
#15044 = CIRCLE ( 'NONE', #14478, 2.055000000000000160 ) ;
#15045 = PRODUCT ( 'torque nut 04-2_iso_ISO 7043-M5-N', 'torque nut 04-2_iso_ISO 7043-M5-N', '', ( #15642 ) ) ;
#15046 = EDGE_LOOP ( 'NONE', ( #14324, #8356, #2180, #8456 ) ) ;
#15047 = CARTESIAN_POINT ( 'NONE',  ( 32.14213199643173624, -2.910415664685331638, 7.939653947423662927 ) ) ;
#15048 = CARTESIAN_POINT ( 'NONE',  ( 28.99445422935450267, -6.424501337975009996, -6.861505862736166250 ) ) ;
#15049 = AXIS2_PLACEMENT_3D ( 'NONE', #15479, #3062, #8582 ) ;
#15050 = CARTESIAN_POINT ( 'NONE',  ( 25.94006848055682113, -4.267777217026356595, -3.719179227265282162 ) ) ;
#15051 = DIRECTION ( 'NONE',  ( 0.8660254037844363761, -0.5000000000000038858, 0.000000000000000000 ) ) ;
#15052 = CARTESIAN_POINT ( 'NONE',  ( 29.50659824675005893, -4.481886499472614638, -7.939653947423662039 ) ) ;
#15053 = DIRECTION ( 'NONE',  ( 0.000000000000000000, 0.000000000000000000, -1.000000000000000000 ) ) ;
#15054 = CARTESIAN_POINT ( 'NONE',  ( 25.76974524478944772, -2.854074692636066946, 6.425565898159212530 ) ) ;
#15055 = EDGE_CURVE ( 'NONE', #15308, #1845, #8298, .T. ) ;
#15056 = CARTESIAN_POINT ( 'NONE',  ( 26.01652455409633902, -4.902371455920926380, -5.783357778048663356 ) ) ;
#15057 = B_SPLINE_CURVE_WITH_KNOTS ( 'NONE', 3,
 ( #12842, #3232, #4845, #1971, #12925, #10373, #14581, #6024, #13201, #14302, #3139, #4672, #777, #6306, #11826, #7493, #14199, #6123 ),
 .UNSPECIFIED., .F., .F.,
 ( 4, 2, 2, 2, 2, 2, 2, 2, 4 ),
 ( 0.000000000000000000, 0.0005710890023745246154, 0.001142178004749049231, 0.001713267007123573955, 0.002284356009498098462, 0.002855445011872622969, 0.003426534014247147909, 0.003997623016621672416, 0.004568712018996196923 ),
 .UNSPECIFIED. ) ;
#15058 = CARTESIAN_POINT ( 'NONE',  ( 28.60033944477555323, -4.591072787911525843, -8.283357778048662468 ) ) ;
#15059 = CARTESIAN_POINT ( 'NONE',  ( 32.77257290155422709, -2.834459985843461816, -3.627061608673662896 ) ) ;
#15060 = ADVANCED_FACE ( 'NONE', ( #6851 ), #9472, .T. ) ;
#15061 = SURFACE_STYLE_FILL_AREA ( #6896 ) ;
#15062 = CARTESIAN_POINT ( 'NONE',  ( 26.56758885001203652, -2.317900097157796324, -5.783357778048670461 ) ) ;
#15063 = CARTESIAN_POINT ( 'NONE',  ( 1.296864337298335788E-21, -1.182044466681725685E-21, -6.899999999999998579 ) ) ;
#15064 = DIRECTION ( 'NONE',  ( 0.9928203230275510771, 0.1196152422706614621, -0.000000000000000000 ) ) ;
#15065 = AXIS2_PLACEMENT_3D ( 'NONE', #2210, #477, #17081 ) ;
#15066 = CARTESIAN_POINT ( 'NONE',  ( 28.75786045390062995, -2.691183018653962034, -6.861505862736159145 ) ) ;
#15067 = EDGE_CURVE ( 'NONE', #5433, #4593, #7015, .T. ) ;
#15068 = AXIS2_PLACEMENT_3D ( 'NONE', #342, #5032, #13204 ) ;
#15069 = AXIS2_PLACEMENT_3D ( 'NONE', #381, #11410, #3815 ) ;
#15070 = CARTESIAN_POINT ( 'NONE',  ( 35.74085044863416982, 7.999999999999934275, 11.27079897466147429 ) ) ;
#15071 = EDGE_LOOP ( 'NONE', ( #16563, #7498, #17357, #1117 ) ) ;
#15072 = VERTEX_POINT ( 'NONE', #3785 ) ;
#15073 = CIRCLE ( 'NONE', #17436, 0.9000000000000003553 ) ;
#15074 = EDGE_CURVE ( 'NONE', #9208, #16590, #9307, .T. ) ;
#15075 = CARTESIAN_POINT ( 'NONE',  ( 28.40332666278570173, -4.614808937445885384, -7.939653947423662039 ) ) ;
#15076 =( GEOMETRIC_REPRESENTATION_CONTEXT ( 3 ) GLOBAL_UNCERTAINTY_ASSIGNED_CONTEXT ( ( #6809 ) ) GLOBAL_UNIT_ASSIGNED_CONTEXT ( ( #9663, #8057, #12493 ) ) REPRESENTATION_CONTEXT ( 'NONE', 'WORKASPACE' ) );
#15077 = VERTEX_POINT ( 'NONE', #11363 ) ;
#15078 = PLANE ( 'NONE',  #4678 ) ;
#15079 = VERTEX_POINT ( 'NONE', #13918 ) ;
#15080 = CARTESIAN_POINT ( 'NONE',  ( 33.38562051666750818, -5.268481986227246061, -7.939653947423664704 ) ) ;
#15081 = AXIS2_PLACEMENT_3D ( 'NONE', #10331, #11612, #17365 ) ;
#15082 = CARTESIAN_POINT ( 'NONE',  ( 31.75254397038802878, -4.211294393702175398, 3.283357778048664244 ) ) ;
#15083 = CARTESIAN_POINT ( 'NONE',  ( 4.211399264691416455, -2.459727859270661288, -3.451161839612817861 ) ) ;
#15084 = CIRCLE ( 'NONE', #7573, 2.499999999999998668 ) ;
#15085 = CARTESIAN_POINT ( 'NONE',  ( 27.26074174026764751, -6.633379454790151009, -6.861505862736167138 ) ) ;
#15086 = ORIENTED_EDGE ( 'NONE', *, *, #15067, .F. ) ;
#15087 = CARTESIAN_POINT ( 'NONE',  ( 19.23308179030308551, -21.22208063239337505, -15.64628783324453387 ) ) ;
#15088 = VECTOR ( 'NONE', #7527, 1000.000000000000000 ) ;
#15089 = EDGE_CURVE ( 'NONE', #14093, #254, #16585, .T. ) ;
#15090 = CARTESIAN_POINT ( 'NONE',  ( 31.24031073583692475, -4.273008382657478954, 7.939653947423662039 ) ) ;
#15091 = CARTESIAN_POINT ( 'NONE',  ( -20.25000000000001066, -16.21813761408365195, -13.00000000000000355 ) ) ;
#15092 = VERTEX_POINT ( 'NONE', #3224 ) ;
#15093 = VECTOR ( 'NONE', #11268, 1000.000000000000227 ) ;
#15094 = ORIENTED_EDGE ( 'NONE', *, *, #3962, .F. ) ;
#15095 = DIRECTION ( 'NONE',  ( -0.1196152422706611984, 0.9928203230275510771, 0.000000000000000000 ) ) ;
#15096 = DIRECTION ( 'NONE',  ( -0.5000000000000099920, -0.8660254037844329345, 0.000000000000000000 ) ) ;
#15097 = CARTESIAN_POINT ( 'NONE',  ( 28.28502977505876359, -2.748149777785362957, -6.861505862736158257 ) ) ;
#15098 = AXIS2_PLACEMENT_3D ( 'NONE', #1283, #6805, #2731 ) ;
#15099 = CARTESIAN_POINT ( 'NONE',  ( -4.000000000000000000, -2.309401076758510918, -0.5000000000000000000 ) ) ;
#15100 = CARTESIAN_POINT ( 'NONE',  ( 27.81599742762458050, -2.504850134108091098, 4.533357778048667797 ) ) ;
#15101 = DIRECTION ( 'NONE',  ( -5.026720092345834817E-22, 4.581671729415426121E-22, 1.000000000000000000 ) ) ;
#15102 = CARTESIAN_POINT ( 'NONE',  ( 27.50150540219088313, -5.977401655418042914, 7.939653947423658487 ) ) ;
#15103 = CARTESIAN_POINT ( 'NONE',  ( 29.99682221560115991, -1.914942061115552541, 5.783357778048668685 ) ) ;
#15104 = DIRECTION ( 'NONE',  ( 0.000000000000000000, -0.5000000000000011102, -0.8660254037844379305 ) ) ;
#15105 = DIRECTION ( 'NONE',  ( -0.000000000000000000, -0.000000000000000000, 1.000000000000000000 ) ) ;
#15106 = AXIS2_PLACEMENT_3D ( 'NONE', #12485, #15293, #71 ) ;
#15107 = CARTESIAN_POINT ( 'NONE',  ( 33.35047706458318828, -2.764833946905071560, 3.627061608673666893 ) ) ;
#15108 = ADVANCED_FACE ( 'NONE', ( #1882 ), #16882, .T. ) ;
#15109 = EDGE_LOOP ( 'NONE', ( #6455, #1938, #15306, #16730 ) ) ;
#15110 = EDGE_CURVE ( 'NONE', #8113, #17858, #5657, .T. ) ;
#15111 = VECTOR ( 'NONE', #2483, 1000.000000000000000 ) ;
#15112 = ORIENTED_EDGE ( 'NONE', *, *, #5421, .T. ) ;
#15113 = CARTESIAN_POINT ( 'NONE',  ( 30.23341599105502908, -5.648260380436597394, 3.627061608673662896 ) ) ;
#15114 = CYLINDRICAL_SURFACE ( 'NONE', #3259, 2.749999999999992006 ) ;
#15115 = ORIENTED_EDGE ( 'NONE', *, *, #13251, .F. ) ;
#15116 = CARTESIAN_POINT ( 'NONE',  ( 29.04699097144805364, -6.418171698071525100, 6.861505862736157368 ) ) ;
#15117 =( BOUNDED_CURVE ( )  B_SPLINE_CURVE ( 2, ( #15853, #3787, #7957, #14767, #3425, #17423, #10569, #13218, #2175 ),
 .UNSPECIFIED., .F., .T. ) 
 B_SPLINE_CURVE_WITH_KNOTS ( ( 3, 2, 2, 2, 3 ),
 ( 0.2115384615384615641, 0.2179487179487179516, 0.2307692307692307820, 0.2435897435897435848, 0.2500000000000000000 ),
 .UNSPECIFIED. ) 
 CURVE ( )  GEOMETRIC_REPRESENTATION_ITEM ( )  RATIONAL_B_SPLINE_CURVE ( ( 0.9330127018922194093, 0.9330127018922196314, 1.000000000000000000, 0.8660254037844387076, 1.000000000000000000, 0.8660254037844387076, 1.000000000000000000, 0.9330127018922191873, 0.9330127018922194093 ) ) 
 REPRESENTATION_ITEM ( '' )  );
#15118 = DIRECTION ( 'NONE',  ( 0.1196152422706597829, -0.9928203230275514102, 0.000000000000000000 ) ) ;
#15119 = DIRECTION ( 'NONE',  ( -0.000000000000000000, -0.000000000000000000, -1.000000000000000000 ) ) ;
#15120 = CARTESIAN_POINT ( 'NONE',  ( 33.73390066541284682, -2.518766455766908940, -3.283357778048662023 ) ) ;
#15121 = CARTESIAN_POINT ( 'NONE',  ( 27.78610916120306129, -6.570083055755264745, -4.705209693361169343 ) ) ;
#15122 = LINE ( 'NONE', #8231, #5242 ) ;
#15123 = ORIENTED_EDGE ( 'NONE', *, *, #5209, .F. ) ;
#15124 = CARTESIAN_POINT ( 'NONE',  ( 30.12771560522282499, -7.314681293660012074, -5.783357778048669573 ) ) ;
#15125 = CYLINDRICAL_SURFACE ( 'NONE', #11926, 2.500000000000001776 ) ;
#15126 = CARTESIAN_POINT ( 'NONE',  ( 20.27684169284606241, -10.57794632788464995, -15.46227570229628689 ) ) ;
#15127 = CARTESIAN_POINT ( 'NONE',  ( -10.27627944162877505, 4.200961894323461010, -2.000000000000000000 ) ) ;
#15128 =( NAMED_UNIT ( * ) PLANE_ANGLE_UNIT ( ) SI_UNIT ( $, .RADIAN. ) );
#15129 = ORIENTED_EDGE ( 'NONE', *, *, #10347, .T. ) ;
#15130 = AXIS2_PLACEMENT_3D ( 'NONE', #6585, #9557, #5478 ) ;
#15131 = VECTOR ( 'NONE', #1463, 1000.000000000000000 ) ;
#15132 = CARTESIAN_POINT ( 'NONE',  ( 27.67650891848073158, -3.448435056481901295, -7.939653947423660263 ) ) ;
#15133 = CARTESIAN_POINT ( 'NONE',  ( 27.02414796481377124, -2.900061135469103490, -6.861505862736158257 ) ) ;
#15134 = ORIENTED_EDGE ( 'NONE', *, *, #13805, .F. ) ;
#15135 = CARTESIAN_POINT ( 'NONE',  ( 26.14456121274580624, -5.685614013951941992, 3.283357778048664688 ) ) ;
#15136 = DIRECTION ( 'NONE',  ( 1.000000000000000000, 0.000000000000000000, 0.000000000000000000 ) ) ;
#15137 = AXIS2_PLACEMENT_3D ( 'NONE', #10107, #4412, #9925 ) ;
#15138 = EDGE_CURVE ( 'NONE', #12549, #3497, #2955, .T. ) ;
#15139 = ORIENTED_EDGE ( 'NONE', *, *, #12170, .T. ) ;
#15140 = CARTESIAN_POINT ( 'NONE',  ( 33.40301380667672504, -2.758504307001591993, 7.939653947423662927 ) ) ;
#15141 = AXIS2_PLACEMENT_3D ( 'NONE', #17293, #13367, #3485 ) ;
#15142 = CARTESIAN_POINT ( 'NONE',  ( 29.62036837594175154, -3.214238380052812261, -3.627061608673662896 ) ) ;
#15143 =( BOUNDED_CURVE ( )  B_SPLINE_CURVE ( 2, ( #11289, #16866, #4514, #14127, #1718, #5867, #11391, #16957, #15577 ),
 .UNSPECIFIED., .F., .T. ) 
 B_SPLINE_CURVE_WITH_KNOTS ( ( 3, 2, 2, 2, 3 ),
 ( 0.8269230769230769829, 0.8333333333333333703, 0.8461538461538461453, 0.8589743589743589203, 0.8653846153846154188 ),
 .UNSPECIFIED. ) 
 CURVE ( )  GEOMETRIC_REPRESENTATION_ITEM ( )  RATIONAL_B_SPLINE_CURVE ( ( 0.9330127018922192983, 0.9330127018922198534, 1.000000000000000000, 0.8660254037844387076, 1.000000000000000000, 0.8660254037844387076, 1.000000000000000000, 0.9330127018922187432, 0.9330127018922192983 ) ) 
 REPRESENTATION_ITEM ( '' )  );
#15144 = CARTESIAN_POINT ( 'NONE',  ( 33.68284756902015431, -1.652629194728084450, -1.783357778048662912 ) ) ;
#15145 = DIRECTION ( 'NONE',  ( 0.9928203230275510771, 0.1196152422706609902, 4.006172263299092517E-17 ) ) ;
#15146 = CARTESIAN_POINT ( 'NONE',  ( 29.49337484321020497, -2.602568060005117090, -4.705209693361161349 ) ) ;
#15147 = CARTESIAN_POINT ( 'NONE',  ( 32.58190297908952004, -5.565186596593329149, 3.283357778048663356 ) ) ;
#15148 = ADVANCED_FACE ( 'NONE', ( #14104 ), #10005, .F. ) ;
#15149 = CARTESIAN_POINT ( 'NONE',  ( 13.00000000000000178, 0.000000000000000000, -12.00000000000000000 ) ) ;
#15150 = DIRECTION ( 'NONE',  ( 1.000000000000000000, 0.000000000000000000, 0.000000000000000000 ) ) ;
#15151 = VECTOR ( 'NONE', #2102, 1000.000000000000114 ) ;
#15152 = CARTESIAN_POINT ( 'NONE',  ( 29.38468146192651886, -6.677295441714964142, -7.033357778048666908 ) ) ;
#15153 = ORIENTED_EDGE ( 'NONE', *, *, #7404, .T. ) ;
#15154 = PRESENTATION_LAYER_ASSIGNMENT (  '', '', ( #13706 ) ) ;
#15155 = CARTESIAN_POINT ( 'NONE',  ( 33.40301380667672504, -2.758504307001591549, -3.627061608673662896 ) ) ;
#15156 = CARTESIAN_POINT ( 'NONE',  ( 26.31556265977298992, -7.384422263489805793, -5.783357778048663356 ) ) ;
#15157 = CARTESIAN_POINT ( 'NONE',  ( -25.11802603177690330, -19.03270077640483038, -0.5379818257722508434 ) ) ;
#15158 = CARTESIAN_POINT ( 'NONE',  ( 30.80688261270428541, -4.325227911964988792, 8.283357778048662468 ) ) ;
#15159 = CARTESIAN_POINT ( 'NONE',  ( 25.92467471225709374, -2.732717170633701453, -7.033357778048658027 ) ) ;
#15160 = CARTESIAN_POINT ( 'NONE',  ( 27.72904566057427189, -3.442105416578421284, -3.627061608673662896 ) ) ;
#15161 = EDGE_CURVE ( 'NONE', #10572, #12285, #8387, .T. ) ;
#15162 = ORIENTED_EDGE ( 'NONE', *, *, #14289, .T. ) ;
#15163 = CARTESIAN_POINT ( 'NONE',  ( 32.60321786976872005, -6.626883982076972934, -5.783357778048663356 ) ) ;
#15164 = DIRECTION ( 'NONE',  ( 0.000000000000000000, 0.000000000000000000, -1.000000000000000000 ) ) ;
#15165 = CIRCLE ( 'NONE', #6181, 2.041999999999999815 ) ;
#15166 = CARTESIAN_POINT ( 'NONE',  ( 0.000000000000000000, 0.000000000000000000, 2.399999999999999467 ) ) ;
#15167 = EDGE_CURVE ( 'NONE', #8906, #11992, #14194, .T. ) ;
#15168 = ORIENTED_EDGE ( 'NONE', *, *, #7915, .F. ) ;
#15169 = ADVANCED_FACE ( 'NONE', ( #7047 ), #1690, .F. ) ;
#15170 = CARTESIAN_POINT ( 'NONE',  ( 31.43723430067123914, -2.368371383576012956, -6.861505862736158257 ) ) ;
#15171 = EDGE_LOOP ( 'NONE', ( #5706, #9944, #11442, #12143, #452 ) ) ;
#15172 = DIRECTION ( 'NONE',  ( 0.000000000000000000, 1.000000000000000000, 0.000000000000000000 ) ) ;
#15173 = CARTESIAN_POINT ( 'NONE',  ( 32.01513846370018967, -2.298745344637636912, -4.705209693361161349 ) ) ;
#15174 = DIRECTION ( 'NONE',  ( 0.000000000000000000, 0.000000000000000000, 1.000000000000000000 ) ) ;
#15175 = CARTESIAN_POINT ( 'NONE',  ( 32.60321786976872005, -6.626883982076972046, 5.783357778048664244 ) ) ;
#15176 = CARTESIAN_POINT ( 'NONE',  ( 28.28955653359400557, -5.882457056865704637, -3.627061608673668225 ) ) ;
#15177 = AXIS2_PLACEMENT_3D ( 'NONE', #13716, #15244, #1297 ) ;
#15178 = ORIENTED_EDGE ( 'NONE', *, *, #480, .F. ) ;
#15179 = CARTESIAN_POINT ( 'NONE',  ( 27.02414796481377124, -2.900061135469103490, 4.705209693361168455 ) ) ;
#15180 = CARTESIAN_POINT ( 'NONE',  ( -17.31608032955932330, -13.61075944537037508, 15.95276485144012035 ) ) ;
#15181 = CARTESIAN_POINT ( 'NONE',  ( -2.016448651773435938E-27, -20.49999999999999645, -13.00000000000000355 ) ) ;
#15182 = VERTEX_POINT ( 'NONE', #9726 ) ;
#15183 = CARTESIAN_POINT ( 'NONE',  ( 30.95252083063564896, -1.789602389065743981, 5.113484796970861446 ) ) ;
#15184 = VERTEX_POINT ( 'NONE', #14295 ) ;
#15185 = DIRECTION ( 'NONE',  ( 0.000000000000000000, 0.000000000000000000, -1.000000000000000000 ) ) ;
#15186 = CARTESIAN_POINT ( 'NONE',  ( 26.01652455409633902, -4.902371455920926380, -5.783357778048663356 ) ) ;
#15187 = CARTESIAN_POINT ( 'NONE',  ( 31.56875459193803124, -6.114348982704044921, -4.705209693361169343 ) ) ;
#15188 = UNCERTAINTY_MEASURE_WITH_UNIT (LENGTH_MEASURE( 1.000000000000000082E-05 ), #14598, 'distance_accuracy_value', 'NONE');
#15189 = EDGE_CURVE ( 'NONE', #1069, #12118, #1235, .T. ) ;
#15190 = DIRECTION ( 'NONE',  ( -1.000000000000000000, 0.000000000000000000, 0.000000000000000000 ) ) ;
#15191 = DIRECTION ( 'NONE',  ( 1.000000000000000000, 0.000000000000000000, 0.000000000000000000 ) ) ;
#15192 = CARTESIAN_POINT ( 'NONE',  ( 0.000000000000000000, 0.000000000000000000, -3.700000000000000178 ) ) ;
#15193 = PRODUCT_DEFINITION_SHAPE ( 'NONE', 'NONE',  #817 ) ;
#15194 = CARTESIAN_POINT ( 'NONE',  ( 30.45225960443380231, -4.367952981209816343, 7.939653947423662039 ) ) ;
#15195 = LINE ( 'NONE', #10824, #10186 ) ;
#15196 = DIRECTION ( 'NONE',  ( -1.000000000000000000, 0.000000000000000000, 0.000000000000000000 ) ) ;
#15197 = CARTESIAN_POINT ( 'NONE',  ( 33.56062403295735663, -2.739515387291124426, 7.939653947423664704 ) ) ;
#15198 = ORIENTED_EDGE ( 'NONE', *, *, #9588, .T. ) ;
#15199 = EDGE_LOOP ( 'NONE', ( #266, #5578, #17498 ) ) ;
#15200 = CARTESIAN_POINT ( 'NONE',  ( 29.38830135902312080, -2.615227339812091767, 4.705209693361167567 ) ) ;
#15201 = DIRECTION ( 'NONE',  ( -0.1196152422706584506, 0.9928203230275515212, 0.000000000000000000 ) ) ;
#15202 = ORIENTED_EDGE ( 'NONE', *, *, #1880, .F. ) ;
#15203 = CARTESIAN_POINT ( 'NONE',  ( 27.04606801335823718, -3.524390735323771118, 3.627061608673666449 ) ) ;
#15204 = DIRECTION ( 'NONE',  ( 0.000000000000000000, 0.000000000000000000, -1.000000000000000000 ) ) ;
#15205 = DIRECTION ( 'NONE',  ( -0.000000000000000000, -0.000000000000000000, -1.000000000000000000 ) ) ;
#15207 = FACE_OUTER_BOUND ( 'NONE', #12050, .T. ) ;
#15206 =( GEOMETRIC_REPRESENTATION_CONTEXT ( 3 ) GLOBAL_UNCERTAINTY_ASSIGNED_CONTEXT ( ( #10992 ) ) GLOBAL_UNIT_ASSIGNED_CONTEXT ( ( #13485, #9385, #13655 ) ) REPRESENTATION_CONTEXT ( 'NONE', 'WORKASPACE' ) );
#15208 = CARTESIAN_POINT ( 'NONE',  ( 27.23882169172318513, -6.009049854935478052, -7.939653947423664704 ) ) ;
#15209 = CARTESIAN_POINT ( 'NONE',  ( 28.76917853929504432, -3.116917426439186123, -3.283357778048662023 ) ) ;
#15210 = DIRECTION ( 'NONE',  ( 1.224646799147353207E-16, 1.000000000000000000, 0.000000000000000000 ) ) ;
#15211 = EDGE_CURVE ( 'NONE', #2920, #15079, #12562, .T. ) ;
#15212 = CARTESIAN_POINT ( 'NONE',  ( 2.805705207896067144, -3.226868319750166858, -3.203898532754369644 ) ) ;
#15213 = CARTESIAN_POINT ( 'NONE',  ( 8.874038404635943067, -3.391377654146811693, -2.000000000000000000 ) ) ;
#15214 = ORIENTED_EDGE ( 'NONE', *, *, #6280, .F. ) ;
#15215 = CARTESIAN_POINT ( 'NONE',  ( 29.14753769709988518, -3.271205139184214516, -3.627061608673662008 ) ) ;
#15216 = CARTESIAN_POINT ( 'NONE',  ( 28.71854711534694715, -4.576831098024959132, -3.627061608673664672 ) ) ;
#15217 = DIRECTION ( 'NONE',  ( 0.000000000000000000, 1.000000000000000000, 0.000000000000000000 ) ) ;
#15218 = FACE_OUTER_BOUND ( 'NONE', #2264, .T. ) ;
#15219 = ORIENTED_EDGE ( 'NONE', *, *, #8106, .F. ) ;
#15220 = EDGE_LOOP ( 'NONE', ( #4710, #11741, #12280, #4350 ) ) ;
#15221 = EDGE_LOOP ( 'NONE', ( #5622, #3571 ) ) ;
#15222 =( BOUNDED_CURVE ( )  B_SPLINE_CURVE ( 2, ( #2435, #17693, #10735, #16309, #2510, #144, #2956, #7225, #9823 ),
 .UNSPECIFIED., .F., .T. ) 
 B_SPLINE_CURVE_WITH_KNOTS ( ( 3, 2, 2, 2, 3 ),
 ( 0.2884615384615384914, 0.2948717948717948789, 0.3076923076923077094, 0.3205128205128205399, 0.3269230769230769273 ),
 .UNSPECIFIED. ) 
 CURVE ( )  GEOMETRIC_REPRESENTATION_ITEM ( )  RATIONAL_B_SPLINE_CURVE ( ( 0.9330127018922194093, 0.9330127018922196314, 1.000000000000000000, 0.8660254037844387076, 1.000000000000000000, 0.8660254037844387076, 1.000000000000000000, 0.9330127018922194093, 0.9330127018922194093 ) ) 
 REPRESENTATION_ITEM ( '' )  );
#15223 = PRODUCT_DEFINITION ( 'UNKNOWN', '', #5985, #8804 ) ;
#15224 = ORIENTED_EDGE ( 'NONE', *, *, #6072, .T. ) ;
#15225 = CARTESIAN_POINT ( 'NONE',  ( 30.88125018618674034, -3.062327022369072171, 7.939653947423662927 ) ) ;
#15226 = CARTESIAN_POINT ( 'NONE',  ( 31.43732351782677625, -4.249272233123119413, 8.283357778048662468 ) ) ;
#15227 = CARTESIAN_POINT ( 'NONE',  ( -15.92260893619738837, -28.39189527176317540, -6.000000000000000000 ) ) ;
#15228 = DIRECTION ( 'NONE',  ( -0.000000000000000000, -1.000000000000000000, -0.000000000000000000 ) ) ;
#15229 = CARTESIAN_POINT ( 'NONE',  ( 29.45101334415624095, -7.006662376286321603, -5.783357778048657138 ) ) ;
#15230 = CARTESIAN_POINT ( 'NONE',  ( 30.15026255541241440, -6.285249260098253465, -4.705209693361168455 ) ) ;
#15231 = CARTESIAN_POINT ( 'NONE',  ( -25.11802603177690330, -19.03270077640482683, 10.53798182577225084 ) ) ;
#15232 = CYLINDRICAL_SURFACE ( 'NONE', #1476, 2.500000000000001776 ) ;
#15233 = CARTESIAN_POINT ( 'NONE',  ( 27.17934203385504333, -30.00000000000000355, -13.93658524716016878 ) ) ;
#15234 = CARTESIAN_POINT ( 'NONE',  ( 26.66018910156667232, -2.644102211984857842, -4.533357778048659803 ) ) ;
#15235 = EDGE_LOOP ( 'NONE', ( #9445, #1542, #3882, #125, #10786, #14432, #8288, #5536, #11918, #12073, #5991, #5419, #1133, #6584, #8726 ) ) ;
#15236 = CARTESIAN_POINT ( 'NONE',  ( 31.27962407439061110, -2.387360303286481855, -6.861505862736159145 ) ) ;
#15237 = DIRECTION ( 'NONE',  ( 1.000000000000000000, 0.000000000000000000, 0.000000000000000000 ) ) ;
#15238 = CARTESIAN_POINT ( 'NONE',  ( -23.00000000000000000, -16.21813761408365195, -13.00000000000000355 ) ) ;
#15239 = FACE_OUTER_BOUND ( 'NONE', #207, .T. ) ;
#15240 = CARTESIAN_POINT ( 'NONE',  ( 27.50150540219088313, -5.977401655418041138, -3.627061608673667781 ) ) ;
#15241 =( BOUNDED_CURVE ( )  B_SPLINE_CURVE ( 2, ( #303, #5813, #8637, #4287, #12446, #32, #14167, #121, #5541 ),
 .UNSPECIFIED., .F., .T. ) 
 B_SPLINE_CURVE_WITH_KNOTS ( ( 3, 2, 2, 2, 3 ),
 ( 0.4423076923076923461, 0.4487179487179487336, 0.4615384615384615641, 0.4743589743589743390, 0.4807692307692307820 ),
 .UNSPECIFIED. ) 
 CURVE ( )  GEOMETRIC_REPRESENTATION_ITEM ( )  RATIONAL_B_SPLINE_CURVE ( ( 0.9330127018922194093, 0.9330127018922196314, 1.000000000000000000, 0.8660254037844387076, 1.000000000000000000, 0.8660254037844387076, 1.000000000000000000, 0.9330127018922190762, 0.9330127018922194093 ) ) 
 REPRESENTATION_ITEM ( '' )  );
#15242 = ORIENTED_EDGE ( 'NONE', *, *, #7066, .T. ) ;
#15243 = ORIENTED_EDGE ( 'NONE', *, *, #10507, .T. ) ;
#15244 = DIRECTION ( 'NONE',  ( -0.000000000000000000, -0.000000000000000000, 1.000000000000000000 ) ) ;
#15245 = CARTESIAN_POINT ( 'NONE',  ( -1.500000000000000000, 10.39230484541326227, -3.000000000000000000 ) ) ;
#15246 = DIRECTION ( 'NONE',  ( -0.000000000000000000, -1.000000000000000000, 3.469446951953614189E-16 ) ) ;
#15247 = VERTEX_POINT ( 'NONE', #16740 ) ;
#15248 = CARTESIAN_POINT ( 'NONE',  ( 31.55553118839817728, -4.235030543236534939, -7.939653947423662039 ) ) ;
#15249 = CARTESIAN_POINT ( 'NONE',  ( -8.632250723006722026, -18.84644399697197770, -16.84735068286508763 ) ) ;
#15250 =( BOUNDED_CURVE ( )  B_SPLINE_CURVE ( 2, ( #15568, #9933, #3065, #12581, #161 ),
 .UNSPECIFIED., .F., .F. ) 
 B_SPLINE_CURVE_WITH_KNOTS ( ( 3, 2, 3 ),
 ( 0.000000000000000000, 0.01282051282051282007, 0.01923076923076924918 ),
 .UNSPECIFIED. ) 
 CURVE ( )  GEOMETRIC_REPRESENTATION_ITEM ( )  RATIONAL_B_SPLINE_CURVE ( ( 1.000000000000000000, 0.8660254037844387076, 1.000000000000000000, 0.9330127018922191873, 0.9330127018922194093 ) ) 
 REPRESENTATION_ITEM ( '' )  );
#15251 = EDGE_CURVE ( 'NONE', #8853, #13220, #5845, .T. ) ;
#15252 = ORIENTED_EDGE ( 'NONE', *, *, #15614, .T. ) ;
#15253 = CARTESIAN_POINT ( 'NONE',  ( 30.75425665345519732, -2.450656702321377001, -4.705209693361161349 ) ) ;
#15254 = CARTESIAN_POINT ( 'NONE',  ( 45.00000000000000711, -16.03270077640482683, -5.537981825772250843 ) ) ;
#15255 = CARTESIAN_POINT ( 'NONE',  ( 32.60321786976872005, -6.626883982076972934, 5.783357778048664244 ) ) ;
#15256 = CARTESIAN_POINT ( 'NONE',  ( 25.99533317148741318, -3.650983533393564517, -3.627061608673662008 ) ) ;
#15257 = CARTESIAN_POINT ( 'NONE',  ( 28.69037342443288452, -3.126411886501869741, 8.283357778048666020 ) ) ;
#15258 = ORIENTED_EDGE ( 'NONE', *, *, #8527, .F. ) ;
#15259 = EDGE_CURVE ( 'NONE', #17725, #12450, #12231, .T. ) ;
#15260 = SURFACE_STYLE_USAGE ( .BOTH. , #1177 ) ;
#15261 = AXIS2_PLACEMENT_3D ( 'NONE', #487, #4470, #17000 ) ;
#15262 = CARTESIAN_POINT ( 'NONE',  ( 0.000000000000000000, 0.000000000000000000, 8.700000000000001066 ) ) ;
#15263 = CARTESIAN_POINT ( 'NONE',  ( 35.41536221060850664, -16.03270077640482683, 10.53798182577225084 ) ) ;
#15264 = ORIENTED_EDGE ( 'NONE', *, *, #1824, .T. ) ;
#15265 =( NAMED_UNIT ( * ) SI_UNIT ( $, .STERADIAN. ) SOLID_ANGLE_UNIT ( ) );
#15266 = ORIENTED_EDGE ( 'NONE', *, *, #7422, .T. ) ;
#15267 = EDGE_LOOP ( 'NONE', ( #3697, #11658, #14867, #8417 ) ) ;
#15268 = ORIENTED_EDGE ( 'NONE', *, *, #11541, .T. ) ;
#15269 = DIRECTION ( 'NONE',  ( 1.000000000000000000, 0.000000000000000000, -0.000000000000000000 ) ) ;
#15270 = CARTESIAN_POINT ( 'NONE',  ( 25.96860978910007844, -6.167287525404733017, -7.540302725459484989 ) ) ;
#15271 = ADVANCED_FACE ( 'NONE', ( #11259 ), #9822, .F. ) ;
#15272 = CARTESIAN_POINT ( 'NONE',  ( -3.436326524993698062, 2.634838109288787145, -3.231543764077259517 ) ) ;
#15273 = CARTESIAN_POINT ( 'NONE',  ( 28.82057243903374655, -7.082618055128190093, -5.783357778048668685 ) ) ;
#15274 = DIRECTION ( 'NONE',  ( 1.000000000000000000, 0.000000000000000000, 0.000000000000000000 ) ) ;
#15275 = CARTESIAN_POINT ( 'NONE',  ( 33.52375369703867847, -2.544085015380856518, 3.283357778048666464 ) ) ;
#15276 = CARTESIAN_POINT ( 'NONE',  ( 30.90769699326644826, -6.820963901304073929, 5.783357778048658027 ) ) ;
#15277 = CIRCLE ( 'NONE', #7469, 2.001963570546864801 ) ;
#15278 = DIRECTION ( 'NONE',  ( 1.000000000000000000, 0.000000000000000000, 0.000000000000000000 ) ) ;
#15279 = CARTESIAN_POINT ( 'NONE',  ( -16.75000000000000000, -16.21813761408365195, 13.00000000000000178 ) ) ;
#15280 = ADVANCED_FACE ( 'NONE', ( #4491 ), #7224, .F. ) ;
#15281 = DIRECTION ( 'NONE',  ( 0.8660254037844432595, 0.4999999999999921174, 0.000000000000000000 ) ) ;
#15282 = ORIENTED_EDGE ( 'NONE', *, *, #17819, .F. ) ;
#15283 = VECTOR ( 'NONE', #12322, 1000.000000000000227 ) ;
#15284 = VERTEX_POINT ( 'NONE', #426 ) ;
#15285 = EDGE_CURVE ( 'NONE', #17574, #11056, #6663, .T. ) ;
#15286 = CARTESIAN_POINT ( 'NONE',  ( 27.71165237056504438, -5.952083095804076684, 3.627061608673662896 ) ) ;
#15287 = DIRECTION ( 'NONE',  ( -1.000000000000000000, 0.000000000000000000, 0.000000000000000000 ) ) ;
#15288 = ORIENTED_EDGE ( 'NONE', *, *, #17191, .T. ) ;
#15289 = CARTESIAN_POINT ( 'NONE',  ( 28.54354359905709160, -7.105797696961086096, 5.783357778048657138 ) ) ;
#15290 = VERTEX_POINT ( 'NONE', #3673 ) ;
#15291 = DIRECTION ( 'NONE',  ( -0.1196152422706610735, 0.9928203230275511881, 0.000000000000000000 ) ) ;
#15292 = CARTESIAN_POINT ( 'NONE',  ( 2.500000000000000000, 0.000000000000000000, 0.000000000000000000 ) ) ;
#15293 = DIRECTION ( 'NONE',  ( -5.026720092345836698E-22, 4.581671729415424240E-22, -1.000000000000000000 ) ) ;
#15294 = CIRCLE ( 'NONE', #17659, 5.500000000000000888 ) ;
#15295 = CARTESIAN_POINT ( 'NONE',  ( 26.19678349485696955, -4.880653813392439311, -3.627061608673664672 ) ) ;
#15296 = CARTESIAN_POINT ( 'NONE',  ( 26.28630169594996246, -7.141552884944044166, -6.905585309297165963 ) ) ;
#15297 = CARTESIAN_POINT ( 'NONE',  ( 30.48043329534786849, -5.818372192732907067, -3.283357778048667797 ) ) ;
#15298 = CARTESIAN_POINT ( 'NONE',  ( 32.52441275490655670, -6.636378442139655220, -5.783357778048663356 ) ) ;
#15299 = EDGE_CURVE ( 'NONE', #17262, #11389, #375, .T. ) ;
#15300 = CARTESIAN_POINT ( 'NONE',  ( 28.40059689994085801, -13.06564623954105464, -13.61006631438115200 ) ) ;
#15301 = CARTESIAN_POINT ( 'NONE',  ( 26.79770707206266778, -11.23794579741151090, 14.03572743982056181 ) ) ;
#15302 = CARTESIAN_POINT ( 'NONE',  ( 31.51621784984448738, -6.120678622607529817, -6.861505862736166250 ) ) ;
#15303 = VERTEX_POINT ( 'NONE', #8846 ) ;
#15304 = AXIS2_PLACEMENT_3D ( 'NONE', #5241, #10762, #16340 ) ;
#15305 = CARTESIAN_POINT ( 'NONE',  ( 28.49970350196817392, -5.857138497251737519, -7.939653947423662927 ) ) ;
#15306 = ORIENTED_EDGE ( 'NONE', *, *, #7943, .F. ) ;
#15307 = VECTOR ( 'NONE', #1322, 1000.000000000000000 ) ;
#15308 = VERTEX_POINT ( 'NONE', #11822 ) ;
#15309 = ORIENTED_EDGE ( 'NONE', *, *, #2471, .F. ) ;
#15310 = ADVANCED_FACE ( 'NONE', ( #4668 ), #4839, .F. ) ;
#15311 = CARTESIAN_POINT ( 'NONE',  ( 28.87615734162756453, -4.557842178314484016, 3.627061608673664228 ) ) ;
#15312 = CIRCLE ( 'NONE', #3750, 10.50000000000000000 ) ;
#15313 = CARTESIAN_POINT ( 'NONE',  ( 31.00882954110335632, -1.782818301463667598, 6.453230759126474148 ) ) ;
#15314 = CARTESIAN_POINT ( 'NONE',  ( -45.00000000000000711, -16.03270077640482683, 10.53798182577225084 ) ) ;
#15315 = CARTESIAN_POINT ( 'NONE',  ( -3.248936832696171617, 17.78798921770683350, -17.00000000000000000 ) ) ;
#15316 = DIRECTION ( 'NONE',  ( 1.000000000000000000, 0.000000000000000000, 0.000000000000000000 ) ) ;
#15317 = CARTESIAN_POINT ( 'NONE',  ( 30.45225960443380231, -4.367952981209816343, -3.627061608673664672 ) ) ;
#15318 = LINE ( 'NONE', #11206, #2934 ) ;
#15319 = LINE ( 'NONE', #15149, #13 ) ;
#15320 = AXIS2_PLACEMENT_3D ( 'NONE', #7993, #13790, #6465 ) ;
#15321 = DIRECTION ( 'NONE',  ( -0.7681011886108269904, -0.5760758914581204371, -0.2795659695588260107 ) ) ;
#15322 = EDGE_CURVE ( 'NONE', #9826, #6903, #6441, .T. ) ;
#15323 = CARTESIAN_POINT ( 'NONE',  ( 27.52714686987067694, -7.627998469090175426, -5.783357778048669573 ) ) ;
#15324 = CARTESIAN_POINT ( 'NONE',  ( 30.12381574833269937, -2.526612381163247267, -4.705209693361161349 ) ) ;
#15325 = CARTESIAN_POINT ( 'NONE',  ( 23.00000000000000000, -16.21813761408365195, -13.00000000000000355 ) ) ;
#15326 = CARTESIAN_POINT ( 'NONE',  ( 33.76207435632690590, -3.969185667289998332, 7.939653947423662039 ) ) ;
#15327 = CARTESIAN_POINT ( 'NONE',  ( 33.60446413004628141, -3.988174587000466342, -3.627061608673664672 ) ) ;
#15328 =( BOUNDED_CURVE ( )  B_SPLINE_CURVE ( 2, ( #5635, #10976, #1669, #13727, #9895, #13998, #17926, #3028, #5458 ),
 .UNSPECIFIED., .F., .T. ) 
 B_SPLINE_CURVE_WITH_KNOTS ( ( 3, 2, 2, 2, 3 ),
 ( 0.5192307692307692735, 0.5256410256410256610, 0.5384615384615384359, 0.5512820512820513219, 0.5576923076923077094 ),
 .UNSPECIFIED. ) 
 CURVE ( )  GEOMETRIC_REPRESENTATION_ITEM ( )  RATIONAL_B_SPLINE_CURVE ( ( 0.9330127018922192983, 0.9330127018922198534, 1.000000000000000000, 0.8660254037844387076, 1.000000000000000000, 0.8660254037844387076, 1.000000000000000000, 0.9330127018922194093, 0.9330127018922194093 ) ) 
 REPRESENTATION_ITEM ( '' )  );
#15329 = CARTESIAN_POINT ( 'NONE',  ( 16.75000000000000000, -16.21813761408365195, -13.00000000000000178 ) ) ;
#15330 = CARTESIAN_POINT ( 'NONE',  ( 32.19529564017040002, -1.250324391365404741, 5.783357778048668685 ) ) ;
#15331 = CARTESIAN_POINT ( 'NONE',  ( 28.34209327568754944, -5.876127416962207306, -7.939653947423662927 ) ) ;
#15332 = VECTOR ( 'NONE', #178, 1000.000000000000000 ) ;
#15333 = EDGE_LOOP ( 'NONE', ( #15986, #7836, #6333, #1753 ) ) ;
#15334 = EDGE_CURVE ( 'NONE', #6838, #12650, #861, .T. ) ;
#15335 = VERTEX_POINT ( 'NONE', #6118 ) ;
#15336 = DIRECTION ( 'NONE',  ( -1.000000000000000000, 0.000000000000000000, 0.000000000000000000 ) ) ;
#15337 = DIRECTION ( 'NONE',  ( 0.000000000000000000, 0.000000000000000000, 1.000000000000000000 ) ) ;
#15338 = CARTESIAN_POINT ( 'NONE',  ( -34.91377932259078420, -11.86950488720510322, -11.57182824616228878 ) ) ;
#15339 = ORIENTED_EDGE ( 'NONE', *, *, #12198, .T. ) ;
#15340 = VECTOR ( 'NONE', #9936, 1000.000000000000227 ) ;
#15341 = CARTESIAN_POINT ( 'NONE',  ( 30.93831368681553684, -6.190304661545915188, -4.705209693361169343 ) ) ;
#15342 = CARTESIAN_POINT ( 'NONE',  ( 7.345582307948228973, 16.91090888051954977, 16.91488491921997195 ) ) ;
#15343 = AXIS2_PLACEMENT_3D ( 'NONE', #4945, #10474, #8947 ) ;
#15344 = VERTEX_POINT ( 'NONE', #7581 ) ;
#15345 = CARTESIAN_POINT ( 'NONE',  ( 29.62489513447700062, -6.348545659133139729, -6.861505862736166250 ) ) ;
#15346 = DIRECTION ( 'NONE',  ( 0.000000000000000000, 0.4999999999999991118, -0.8660254037844391517 ) ) ;
#15347 = CYLINDRICAL_SURFACE ( 'NONE', #16159, 5.000000000000000000 ) ;
#15348 = VERTEX_POINT ( 'NONE', #14575 ) ;
#15349 = CARTESIAN_POINT ( 'NONE',  ( 32.38298487551052318, -4.135338714860305132, -8.283357778048662468 ) ) ;
#15350 =( BOUNDED_CURVE ( )  B_SPLINE_CURVE ( 3, ( #15511, #11598, #1836, #10484 ),
 .UNSPECIFIED., .F., .F. ) 
 B_SPLINE_CURVE_WITH_KNOTS ( ( 4, 4 ),
 ( 1.221730476396036824, 1.230954889131919305 ),
 .UNSPECIFIED. ) 
 CURVE ( )  GEOMETRIC_REPRESENTATION_ITEM ( )  RATIONAL_B_SPLINE_CURVE ( ( 1.000000000000000000, 0.9999929091967096895, 0.9999929091967096895, 1.000000000000000000 ) ) 
 REPRESENTATION_ITEM ( '' )  );
#15351 = ORIENTED_EDGE ( 'NONE', *, *, #8540, .F. ) ;
#15352 = CARTESIAN_POINT ( 'NONE',  ( 21.62682814333776804, -22.31876753225984800, -15.20565444446567227 ) ) ;
#15353 = ORIENTED_EDGE ( 'NONE', *, *, #3672, .F. ) ;
#15354 = CARTESIAN_POINT ( 'NONE',  ( 29.26075783691881682, -2.330785036554694489, 7.033357778048666020 ) ) ;
#15355 = EDGE_CURVE ( 'NONE', #14109, #10285, #4904, .T. ) ;
#15356 = MECHANICAL_DESIGN_GEOMETRIC_PRESENTATION_REPRESENTATION (  '', ( #599 ), #9275 ) ;
#15357 = CARTESIAN_POINT ( 'NONE',  ( 1.500000000000000000, -11.00000000000000000, -2.000000000000000000 ) ) ;
#15358 = CARTESIAN_POINT ( 'NONE',  ( 33.26181313012506280, -6.547536259434060923, 5.113484796970854340 ) ) ;
#15359 = ORIENTED_EDGE ( 'NONE', *, *, #1356, .T. ) ;
#15360 = CARTESIAN_POINT ( 'NONE',  ( 25.11802603177690330, -19.03270077640482683, 10.53798182577225084 ) ) ;
#15361 = ORIENTED_EDGE ( 'NONE', *, *, #2231, .T. ) ;
#15362 = CARTESIAN_POINT ( 'NONE',  ( 26.78782184427022983, -4.809445364374452581, 3.283357778048664244 ) ) ;
#15363 = ORIENTED_EDGE ( 'NONE', *, *, #3123, .T. ) ;
#15364 = DIRECTION ( 'NONE',  ( 1.000000000000000000, 0.000000000000000000, 0.000000000000000000 ) ) ;
#15365 = AXIS2_PLACEMENT_3D ( 'NONE', #7378, #9785, #13885 ) ;
#15366 = AXIS2_PLACEMENT_3D ( 'NONE', #14571, #2149, #9193 ) ;
#15367 = CARTESIAN_POINT ( 'NONE',  ( 27.23882169172318513, -6.009049854935478052, -7.939653947423664704 ) ) ;
#15368 = DIRECTION ( 'NONE',  ( -5.026720092345836698E-22, 4.581671729415424240E-22, -1.000000000000000000 ) ) ;
#15369 = DIRECTION ( 'NONE',  ( 0.000000000000000000, -2.775557561562891351E-17, 1.000000000000000000 ) ) ;
#15370 = CARTESIAN_POINT ( 'NONE',  ( 33.48996557372703364, -1.821249024531260696, 4.533357778048667797 ) ) ;
#15371 = CARTESIAN_POINT ( 'NONE',  ( 31.87075164095941915, -4.197052703815608687, -3.627061608673664672 ) ) ;
#15372 = VECTOR ( 'NONE', #4613, 1000.000000000000000 ) ;
#15373 = DIRECTION ( 'NONE',  ( -0.000000000000000000, -0.000000000000000000, 1.000000000000000000 ) ) ;
#15374 = CARTESIAN_POINT ( 'NONE',  ( 31.84257795004536007, -2.746633492292519296, 8.283357778048666020 ) ) ;
#15375 = CARTESIAN_POINT ( 'NONE',  ( 31.41531425212677675, -1.744041783721344219, 5.783357778048668685 ) ) ;
#15376 = VERTEX_POINT ( 'NONE', #9197 ) ;
#15377 = CIRCLE ( 'NONE', #12764, 9.500000000000000000 ) ;
#15378 = EDGE_CURVE ( 'NONE', #15077, #12431, #2961, .T. ) ;
#15379 = VERTEX_POINT ( 'NONE', #7751 ) ;
#15380 = CARTESIAN_POINT ( 'NONE',  ( 29.41022140756759029, -3.239556939666760726, 3.627061608673666893 ) ) ;
#15381 = CARTESIAN_POINT ( 'NONE',  ( 31.51612863268893960, -4.239777773060436239, -3.283357778048664688 ) ) ;
#15382 = CARTESIAN_POINT ( 'NONE',  ( 1.500000000000000000, -10.05532945112458876, -2.666480854966549074 ) ) ;
#15383 = VERTEX_POINT ( 'NONE', #4754 ) ;
#15384 = CARTESIAN_POINT ( 'NONE',  ( 25.78291734803729796, -2.627872734613073913, 6.136288781622796229 ) ) ;
#15385 = DIRECTION ( 'NONE',  ( -1.000000000000000000, 0.000000000000000000, 0.000000000000000000 ) ) ;
#15386 = VECTOR ( 'NONE', #17010, 1000.000000000000227 ) ;
#15387 = DIRECTION ( 'NONE',  ( 0.9928203230275512992, 0.1196152422706610180, 4.006172263299093133E-17 ) ) ;
#15388 = DIRECTION ( 'NONE',  ( 1.000000000000000000, 0.000000000000000000, 0.000000000000000000 ) ) ;
#15389 = CARTESIAN_POINT ( 'NONE',  ( -10.50000000000000000, 0.000000000000000000, -4.000000000000000000 ) ) ;
#15390 = CARTESIAN_POINT ( 'NONE',  ( 27.38828526237195504, -6.917821758047558056, -4.533357778048668685 ) ) ;
#15391 = EDGE_CURVE ( 'NONE', #16897, #17484, #13195, .T. ) ;
#15392 = CARTESIAN_POINT ( 'NONE',  ( 30.72436838703367812, -6.515889623968540434, -7.033357778048666908 ) ) ;
#15393 = CARTESIAN_POINT ( 'NONE',  ( 26.79666222766753592, -21.19920099154242976, 14.03599807436713398 ) ) ;
#15394 = AXIS2_PLACEMENT_3D ( 'NONE', #7883, #5141, #2447 ) ;
#15395 = DIRECTION ( 'NONE',  ( 0.000000000000000000, 0.000000000000000000, 1.000000000000000000 ) ) ;
#15396 =( NAMED_UNIT ( * ) SI_UNIT ( $, .STERADIAN. ) SOLID_ANGLE_UNIT ( ) );
#15397 = CARTESIAN_POINT ( 'NONE',  ( 30.12381574833269937, -2.526612381163247267, -4.705209693361161349 ) ) ;
#15398 = ORIENTED_EDGE ( 'NONE', *, *, #1087, .T. ) ;
#15399 = VECTOR ( 'NONE', #8677, 1000.000000000000000 ) ;
#15400 = CARTESIAN_POINT ( 'NONE',  ( 26.82722439997946395, -4.804698134550569044, -3.627061608673664672 ) ) ;
#15401 = AXIS2_PLACEMENT_3D ( 'NONE', #1806, #12853, #11746 ) ;
#15402 = DIRECTION ( 'NONE',  ( 1.000000000000000000, 0.000000000000000000, 0.000000000000000000 ) ) ;
#15403 = VECTOR ( 'NONE', #3753, 1000.000000000000227 ) ;
#15404 = ORIENTED_EDGE ( 'NONE', *, *, #2607, .F. ) ;
#15405 = EDGE_LOOP ( 'NONE', ( #16223, #12069 ) ) ;
#15406 = VERTEX_POINT ( 'NONE', #15828 ) ;
#15407 = CARTESIAN_POINT ( 'NONE',  ( 28.76238721243587548, -5.825490297734302381, 7.939653947423658487 ) ) ;
#15408 = VECTOR ( 'NONE', #4321, 1000.000000000000000 ) ;
#15409 = CARTESIAN_POINT ( 'NONE',  ( 26.24062359194589433, -6.129313013101782559, -3.627061608673667781 ) ) ;
#15410 = CARTESIAN_POINT ( 'NONE',  ( 0.000000000000000000, 0.000000000000000000, -3.000000000000000000 ) ) ;
#15411 = CARTESIAN_POINT ( 'NONE',  ( 32.24155699611449677, -1.634298987580965923, -5.783357778048664244 ) ) ;
#15412 = CARTESIAN_POINT ( 'NONE',  ( 33.75714020991769360, -6.487859128256953767, -5.113484796970860558 ) ) ;
#15413 = CARTESIAN_POINT ( 'NONE',  ( 29.19137779418881351, -4.519864338893556877, -3.627061608673664672 ) ) ;
#15414 = CARTESIAN_POINT ( 'NONE',  ( 32.00093131988006689, -6.699447617117800569, -6.453230759126470595 ) ) ;
#15415 = DIRECTION ( 'NONE',  ( 1.000000000000000000, 0.000000000000000000, 0.000000000000000000 ) ) ;
#15416 = AXIS2_PLACEMENT_3D ( 'NONE', #7672, #14382, #14743 ) ;
#15417 = CIRCLE ( 'NONE', #7323, 2.000000000000001776 ) ;
#15418 = CARTESIAN_POINT ( 'NONE',  ( 1.655952806101423924, -3.662737355149043861, -9.025983085941824413E-15 ) ) ;
#15419 = CARTESIAN_POINT ( 'NONE',  ( 27.29063000668916672, -2.568146533142987575, -4.533357778048659803 ) ) ;
#15420 = EDGE_CURVE ( 'NONE', #4895, #16872, #2058, .T. ) ;
#15421 = CARTESIAN_POINT ( 'NONE',  ( 28.77978050244509944, -3.315512618508630993, -7.939653947423660263 ) ) ;
#15422 = DIRECTION ( 'NONE',  ( 0.000000000000000000, 0.000000000000000000, 1.000000000000000000 ) ) ;
#15423 = DIRECTION ( 'NONE',  ( 0.9928203230275511881, 0.1196152422706610735, 9.614813431917827710E-17 ) ) ;
#15424 = CARTESIAN_POINT ( 'NONE',  ( 20.25000000000000355, -16.21813761408365195, 0.000000000000000000 ) ) ;
#15425 = CARTESIAN_POINT ( 'NONE',  ( -34.91600907648203389, -11.88801210197604341, 0.000000000000000000 ) ) ;
#15426 = AXIS2_PLACEMENT_3D ( 'NONE', #17854, #10893, #16462 ) ;
#15427 = CARTESIAN_POINT ( 'NONE',  ( 30.44283453230164227, -2.188368138933637574, 7.033357778048666020 ) ) ;
#15428 = CARTESIAN_POINT ( 'NONE',  ( 28.98992747081926069, -3.290194058894681639, -3.627061608673662896 ) ) ;
#15429 = AXIS2_PLACEMENT_3D ( 'NONE', #17599, #16298, #4946 ) ;
#15430 = ORIENTED_EDGE ( 'NONE', *, *, #14797, .F. ) ;
#15431 = EDGE_CURVE ( 'NONE', #2990, #17907, #6212, .T. ) ;
#15432 = LINE ( 'NONE', #4457, #9628 ) ;
#15433 = FACE_OUTER_BOUND ( 'NONE', #12867, .T. ) ;
#15434 = ORIENTED_EDGE ( 'NONE', *, *, #3039, .T. ) ;
#15435 = CARTESIAN_POINT ( 'NONE',  ( -17.71052479140136526, -12.88256812061772116, -15.89289657457836746 ) ) ;
#15436 = CONICAL_SURFACE ( 'NONE', #17791, 9.500000000000001776, 0.7853981633974465026 ) ;
#15437 = ORIENTED_EDGE ( 'NONE', *, *, #2717, .F. ) ;
#15438 = CARTESIAN_POINT ( 'NONE',  ( 28.08810621022444920, -4.652786776866828511, -3.627061608673664672 ) ) ;
#15439 = AXIS2_PLACEMENT_3D ( 'NONE', #7190, #3016, #2913 ) ;
#15440 = EDGE_CURVE ( 'NONE', #17849, #11176, #11730, .T. ) ;
#15441 = CARTESIAN_POINT ( 'NONE',  ( 29.99682221560115991, -1.914942061115552541, -5.783357778048658027 ) ) ;
#15442 = EDGE_CURVE ( 'NONE', #9693, #14407, #12246, .T. ) ;
#15443 = LINE ( 'NONE', #9622, #16792 ) ;
#15444 = DIRECTION ( 'NONE',  ( 0.6000000000000001998, -0.7999999999999999334, 0.000000000000000000 ) ) ;
#15445 = CARTESIAN_POINT ( 'NONE',  ( 31.56485473504790917, -1.326280070207274564, -5.783357778048658027 ) ) ;
#15446 = CARTESIAN_POINT ( 'NONE',  ( 29.27960797773944179, -6.689954721521948144, 7.033357778048657138 ) ) ;
#15447 = ORIENTED_EDGE ( 'NONE', *, *, #6235, .F. ) ;
#15448 = CARTESIAN_POINT ( 'NONE',  ( 25.84216048658649001, -4.923378882637265974, 8.283357778048662468 ) ) ;
#15449 = CARTESIAN_POINT ( 'NONE',  ( 27.67650891848073158, -3.448435056481901295, 3.627061608673666893 ) ) ;
#15450 = CARTESIAN_POINT ( 'NONE',  ( -28.68370877339674863, -18.82577899785919584, 13.53184763361698906 ) ) ;
#15451 = CARTESIAN_POINT ( 'NONE',  ( 30.00264913441657555, -6.940201157507134511, 5.783357778048669573 ) ) ;
#15452 = VERTEX_POINT ( 'NONE', #17114 ) ;
#15453 = SURFACE_SIDE_STYLE ('',( #3036 ) ) ;
#15454 = ORIENTED_EDGE ( 'NONE', *, *, #4512, .F. ) ;
#15455 = CARTESIAN_POINT ( 'NONE',  ( 8.968924017731504605, -19.12031538047531853, -16.82773324567541451 ) ) ;
#15456 = VERTEX_POINT ( 'NONE', #11545 ) ;
#15457 = CARTESIAN_POINT ( 'NONE',  ( 26.94172295629870462, -6.971623697019761146, -7.033357778048666908 ) ) ;
#15458 = CARTESIAN_POINT ( 'NONE',  ( 33.79776779778399032, -6.145605689821873163, -7.033357778048666908 ) ) ;
#15459 = ADVANCED_FACE ( 'NONE', ( #16023 ), #12821, .T. ) ;
#15460 = CARTESIAN_POINT ( 'NONE',  ( 31.35480929215617252, -6.439933945126671055, -7.033357778048666908 ) ) ;
#15461 = CARTESIAN_POINT ( 'NONE',  ( -5.499998817156067865, -20.49639288455253450, 13.00000000000000178 ) ) ;
#15462 = EDGE_CURVE ( 'NONE', #5433, #14350, #6736, .T. ) ;
#15463 = CARTESIAN_POINT ( 'NONE',  ( 23.00000000000000355, -16.21813761408365195, 17.69999999999999574 ) ) ;
#15464 = FACE_OUTER_BOUND ( 'NONE', #2116, .T. ) ;
#15465 = CARTESIAN_POINT ( 'NONE',  ( 32.69811611091622439, -2.216460025892273311, -6.861505862736158257 ) ) ;
#15466 = ADVANCED_FACE ( 'NONE', ( #13281 ), #2849, .T. ) ;
#15467 = CARTESIAN_POINT ( 'NONE',  ( 0.000000000000000000, -1.178949249685213863, 2.042000000000001148 ) ) ;
#15468 = CARTESIAN_POINT ( 'NONE',  ( 26.47260139170898441, -4.847423203795396596, -3.283357778048664688 ) ) ;
#15469 = CARTESIAN_POINT ( 'NONE',  ( 29.55043834383899437, -5.730545699181964991, 7.939653947423658487 ) ) ;
#15470 = EDGE_LOOP ( 'NONE', ( #3819, #4468, #17330, #15139 ) ) ;
#15471 = ADVANCED_FACE ( 'NONE', ( #2877 ), #8402, .T. ) ;
#15472 = ORIENTED_EDGE ( 'NONE', *, *, #10585, .T. ) ;
#15473 = CARTESIAN_POINT ( 'NONE',  ( 26.87106449706838873, -6.053357334259913181, 7.939653947423658487 ) ) ;
#15474 = CARTESIAN_POINT ( 'NONE',  ( 31.05948030073166066, -1.776715885202022394, -5.783357778048662468 ) ) ;
#15475 = DIRECTION ( 'NONE',  ( -1.000000000000000000, 0.000000000000000000, 0.000000000000000000 ) ) ;
#15476 = VERTEX_POINT ( 'NONE', #15389 ) ;
#15477 = CARTESIAN_POINT ( 'NONE',  ( 26.60838078660069428, -6.085005533777348319, 3.627061608673662896 ) ) ;
#15478 = FACE_OUTER_BOUND ( 'NONE', #2875, .T. ) ;
#15479 = CARTESIAN_POINT ( 'NONE',  ( 0.000000000000000000, 0.000000000000000000, -2.000000000000000000 ) ) ;
#15480 = VERTEX_POINT ( 'NONE', #1169 ) ;
#15481 = DIRECTION ( 'NONE',  ( 1.000000000000000000, 0.000000000000000000, 0.000000000000000000 ) ) ;
#15482 = LINE ( 'NONE', #3149, #13085 ) ;
#15483 = DIRECTION ( 'NONE',  ( 1.000000000000000000, 0.000000000000000000, 0.000000000000000000 ) ) ;
#15484 = ORIENTED_EDGE ( 'NONE', *, *, #15462, .T. ) ;
#15485 = CARTESIAN_POINT ( 'NONE',  ( 33.27602027394517847, -2.146833986953896822, -4.705209693361161349 ) ) ;
#15486 = CARTESIAN_POINT ( 'NONE',  ( 29.25000000000000000, -16.21813761408365195, 13.37255996287876236 ) ) ;
#15487 = LINE ( 'NONE', #8587, #7521 ) ;
#15488 = CARTESIAN_POINT ( 'NONE',  ( 31.71314141467879111, -4.216041623526076698, -3.627061608673664672 ) ) ;
#15489 = ORIENTED_EDGE ( 'NONE', *, *, #13684, .F. ) ;
#15490 = ADVANCED_FACE ( 'NONE', ( #6689 ), #9066, .F. ) ;
#15491 = CARTESIAN_POINT ( 'NONE',  ( 25.80383423833348644, -3.137017275366889901, -7.141595990038014818 ) ) ;
#15492 = CARTESIAN_POINT ( 'NONE',  ( 0.000000000000000000, 0.000000000000000000, -4.700000000000000178 ) ) ;
#15493 = VERTEX_POINT ( 'NONE', #9570 ) ;
#15494 = ADVANCED_FACE ( 'NONE', ( #5318, #10841 ), #16407, .T. ) ;
#15495 = ORIENTED_EDGE ( 'NONE', *, *, #13553, .T. ) ;
#15496 = PRESENTATION_LAYER_ASSIGNMENT (  '', '', ( #6229 ) ) ;
#15497 = CARTESIAN_POINT ( 'NONE',  ( 29.62036837594175154, -3.214238380052812261, 7.939653947423662927 ) ) ;
#15498 = ORIENTED_EDGE ( 'NONE', *, *, #15259, .T. ) ;
#15499 = CARTESIAN_POINT ( 'NONE',  ( 29.27960797773944179, -6.689954721521948144, -4.533357778048668685 ) ) ;
#15500 = CYLINDRICAL_SURFACE ( 'NONE', #14441, 14.00000000000000178 ) ;
#15501 = CARTESIAN_POINT ( 'NONE',  ( -18.96667930129623514, 9.308258642545592210, -15.69246997591053017 ) ) ;
#15502 = CARTESIAN_POINT ( 'NONE',  ( 33.32864623319426300, -4.021405196597508613, -3.283357778048664688 ) ) ;
#15503 = CARTESIAN_POINT ( 'NONE',  ( 31.69574812466957781, -6.726019302751734763, -5.783357778048669573 ) ) ;
#15504 = CARTESIAN_POINT ( 'NONE',  ( 20.25000000000000711, -16.21813761408365195, -13.00000000000000178 ) ) ;
#15505 = CYLINDRICAL_SURFACE ( 'NONE', #2349, 2.500000000000001776 ) ;
#15506 = CARTESIAN_POINT ( 'NONE',  ( -3.999999999999999112, 4.898587196589411843E-16, 1.599999999999998979 ) ) ;
#15507 = UNCERTAINTY_MEASURE_WITH_UNIT (LENGTH_MEASURE( 1.000000000000000082E-05 ), #16275, 'distance_accuracy_value', 'NONE');
#15508 = CARTESIAN_POINT ( 'NONE',  ( 0.000000000000000000, 0.000000000000000000, -3.000000000000002665 ) ) ;
#15509 = CARTESIAN_POINT ( 'NONE',  ( 30.65370992780335868, -5.597623261208691581, -3.627061608673667781 ) ) ;
#15510 = PLANE ( 'NONE',  #15952 ) ;
#15511 = CARTESIAN_POINT ( 'NONE',  ( 35.74085044863416982, -18.73429073671341172, 11.27079897466147251 ) ) ;
#15512 = CARTESIAN_POINT ( 'NONE',  ( 26.27285561281999193, -7.029948842322393254, -4.710679390969556124 ) ) ;
#15513 = ORIENTED_EDGE ( 'NONE', *, *, #15957, .F. ) ;
#15514 = DIRECTION ( 'NONE',  ( -0.000000000000000000, -0.000000000000000000, -1.000000000000000000 ) ) ;
#15515 = CARTESIAN_POINT ( 'NONE',  ( 29.41846958523816724, -7.400131432564565515, 5.783357778048657138 ) ) ;
#15516 = CARTESIAN_POINT ( 'NONE',  ( 26.03917326857634151, -4.899642733102906433, -3.627061608673664672 ) ) ;
#15517 = ORIENTED_EDGE ( 'NONE', *, *, #11765, .T. ) ;
#15518 = CARTESIAN_POINT ( 'NONE',  ( 26.53943449477818106, -2.321292140958837624, 5.113484796970856117 ) ) ;
#15519 = CARTESIAN_POINT ( 'NONE',  ( 0.000000000000000000, 0.000000000000000000, -9.600000000000001421 ) ) ;
#15520 = EDGE_CURVE ( 'NONE', #14075, #4809, #13981, .T. ) ;
#15521 = DIRECTION ( 'NONE',  ( 0.000000000000000000, -0.4999999999999992228, 0.8660254037844390407 ) ) ;
#15522 = VERTEX_POINT ( 'NONE', #15661 ) ;
#15523 = CARTESIAN_POINT ( 'NONE',  ( 25.78291734803729796, -2.627872734613073913, -5.430426774474530482 ) ) ;
#15524 = ORIENTED_EDGE ( 'NONE', *, *, #875, .T. ) ;
#15525 = CARTESIAN_POINT ( 'NONE',  ( 28.87615734162756453, -4.557842178314484016, -7.939653947423662039 ) ) ;
#15526 = CARTESIAN_POINT ( 'NONE',  ( 45.50000000000000000, -16.03270077640482683, -5.537981825772250843 ) ) ;
#15527 = FACE_BOUND ( 'NONE', #10330, .T. ) ;
#15528 = CARTESIAN_POINT ( 'NONE',  ( -45.00000000000000711, -16.03270077640482683, -5.537981825772250843 ) ) ;
#15529 = CARTESIAN_POINT ( 'NONE',  ( 32.82573654529290508, -1.174368712523534475, -5.783357778048658027 ) ) ;
#15530 = CARTESIAN_POINT ( 'NONE',  ( -20.00000000000000000, 7.999999999999996447, -12.00000000000000000 ) ) ;
#15531 = ORIENTED_EDGE ( 'NONE', *, *, #7093, .T. ) ;
#15532 = CARTESIAN_POINT ( 'NONE',  ( 32.14665875496697822, -6.044722943765660439, 4.705209693361160461 ) ) ;
#15533 = EDGE_CURVE ( 'NONE', #7100, #4903, #11054, .T. ) ;
#15534 = DIRECTION ( 'NONE',  ( -1.000000000000000000, -0.000000000000000000, -0.000000000000000000 ) ) ;
#15535 = CARTESIAN_POINT ( 'NONE',  ( 29.18195272205665347, -2.340279496617377664, 7.033357778048666020 ) ) ;
#15536 = VERTEX_POINT ( 'NONE', #17034 ) ;
#15537 = DIRECTION ( 'NONE',  ( 0.000000000000000000, 0.000000000000000000, 1.000000000000000000 ) ) ;
#15538 = ORIENTED_EDGE ( 'NONE', *, *, #3003, .F. ) ;
#15539 = CARTESIAN_POINT ( 'NONE',  ( 10.40000000000000036, 1.273632671113247276E-15, 0.000000000000000000 ) ) ;
#15540 = VERTEX_POINT ( 'NONE', #3333 ) ;
#15541 = CARTESIAN_POINT ( 'NONE',  ( 0.000000000000000000, 5.051668046482832750E-16, -4.000000000000000000 ) ) ;
#15542 = CARTESIAN_POINT ( 'NONE',  ( 26.65222088368961195, -7.333664733486695120, -5.783357778048669573 ) ) ;
#15543 = CARTESIAN_POINT ( 'NONE',  ( 30.88568772756644520, -4.315733451902305617, -3.283357778048664688 ) ) ;
#15544 = CYLINDRICAL_SURFACE ( 'NONE', #12451, 2.500000000000001776 ) ;
#15545 = ADVANCED_FACE ( 'NONE', ( #8778 ), #10210, .T. ) ;
#15546 = APPLICATION_PROTOCOL_DEFINITION ( 'draft international standard', 'automotive_design', 1998, #10804 ) ;
#15547 = FACE_OUTER_BOUND ( 'NONE', #17684, .T. ) ;
#15549 = CARTESIAN_POINT ( 'NONE',  ( 29.52399153675929355, -1.971908820246954130, -5.783357778048658027 ) ) ;
#15548 = PRODUCT_RELATED_PRODUCT_CATEGORY ( 'part', '', ( #9104 ) ) ;
#15550 = LINE ( 'NONE', #8483, #15995 ) ;
#15551 = DIRECTION ( 'NONE',  ( 0.000000000000000000, 1.000000000000000000, -1.103561164596346103E-15 ) ) ;
#15552 = DIRECTION ( 'NONE',  ( -1.000000000000000000, 0.000000000000000000, 0.000000000000000000 ) ) ;
#15553 = CARTESIAN_POINT ( 'NONE',  ( 29.65098506949083301, -2.583579140294649523, 6.861505862736166250 ) ) ;
#15554 = AXIS2_PLACEMENT_3D ( 'NONE', #955, #5191, #13372 ) ;
#15555 = ORIENTED_EDGE ( 'NONE', *, *, #12401, .F. ) ;
#15556 = CARTESIAN_POINT ( 'NONE',  ( 25.77727942049545717, -5.625018267156629115, -7.939653947423662039 ) ) ;
#15557 = ORIENTED_EDGE ( 'NONE', *, *, #9354, .T. ) ;
#15558 = EDGE_CURVE ( 'NONE', #7189, #8269, #14311, .T. ) ;
#15559 = CARTESIAN_POINT ( 'NONE',  ( 29.62036837594175154, -3.214238380052812261, 7.939653947423664704 ) ) ;
#15560 = DIRECTION ( 'NONE',  ( -1.000000000000000000, 0.000000000000000000, 0.000000000000000000 ) ) ;
#15561 = DIRECTION ( 'NONE',  ( -0.1196152422706610735, 0.9928203230275511881, 0.000000000000000000 ) ) ;
#15562 = ORIENTED_EDGE ( 'NONE', *, *, #1087, .F. ) ;
#15563 = CARTESIAN_POINT ( 'NONE',  ( 26.62577407660990758, -3.575027854551694695, 7.939653947423662927 ) ) ;
#15564 = ORIENTED_EDGE ( 'NONE', *, *, #6625, .T. ) ;
#15565 = CARTESIAN_POINT ( 'NONE',  ( -4.000000000000000000, 2.511479357205540275, -3.169254599242374404 ) ) ;
#15566 = CARTESIAN_POINT ( 'NONE',  ( 31.89397184978405519, -6.712334120981523711, -5.783357778048663356 ) ) ;
#15567 = FACE_OUTER_BOUND ( 'NONE', #9888, .T. ) ;
#15568 = CARTESIAN_POINT ( 'NONE',  ( 33.95908713831676096, -3.945449517755638791, -3.283357778048664688 ) ) ;
#15569 = ORIENTED_EDGE ( 'NONE', *, *, #11669, .T. ) ;
#15570 = CARTESIAN_POINT ( 'NONE',  ( 26.06734695949040059, -6.350061944625998933, -3.283357778048667797 ) ) ;
#15571 = CIRCLE ( 'NONE', #12089, 5.500000000000000000 ) ;
#15572 = CARTESIAN_POINT ( 'NONE',  ( 29.08710323061924896, -17.65086537115787380, 13.41876697690134179 ) ) ;
#15573 = DIRECTION ( 'NONE',  ( 0.000000000000000000, 0.000000000000000000, 1.000000000000000000 ) ) ;
#15574 = EDGE_CURVE ( 'NONE', #131, #9563, #1033, .T. ) ;
#15575 = CARTESIAN_POINT ( 'NONE',  ( 32.14665875496697822, -6.044722943765660439, -6.861505862736166250 ) ) ;
#15576 = CARTESIAN_POINT ( 'NONE',  ( 27.02867472334902033, -6.034368414549445170, -3.627061608673668225 ) ) ;
#15577 = CARTESIAN_POINT ( 'NONE',  ( 26.56758885001203652, -2.317900097157796324, -5.783357778048670461 ) ) ;
#15578 = ORIENTED_EDGE ( 'NONE', *, *, #5265, .F. ) ;
#15579 = ORIENTED_EDGE ( 'NONE', *, *, #7902, .F. ) ;
#15580 = AXIS2_PLACEMENT_3D ( 'NONE', #12772, #1725, #8422 ) ;
#15581 = ORIENTED_EDGE ( 'NONE', *, *, #9618, .F. ) ;
#15582 = CARTESIAN_POINT ( 'NONE',  ( 29.01637427789896151, -7.048830937829682064, 5.783357778048658915 ) ) ;
#15583 = AXIS2_PLACEMENT_3D ( 'NONE', #1153, #15105, #9219 ) ;
#15584 = FACE_OUTER_BOUND ( 'NONE', #8732, .T. ) ;
#15585 = CARTESIAN_POINT ( 'NONE',  ( 33.60446413004628141, -3.988174587000466342, -3.627061608673664672 ) ) ;
#15586 = ADVANCED_FACE ( 'NONE', ( #10111 ), #14244, .T. ) ;
#15587 = CARTESIAN_POINT ( 'NONE',  ( -11.90182750357594621, 14.98910623166845646, -16.60584412753037853 ) ) ;
#15588 = CARTESIAN_POINT ( 'NONE',  ( -28.39989834181360706, -19.37183319909320645, -13.61025820885934223 ) ) ;
#15589 = CARTESIAN_POINT ( 'NONE',  ( 33.58707084003705745, -6.498152266226123963, -5.783357778048669573 ) ) ;
#15590 = CARTESIAN_POINT ( 'NONE',  ( 25.90934487712385348, 0.1208734971681838660, 5.783357778048663356 ) ) ;
#15591 = CARTESIAN_POINT ( 'NONE',  ( 27.53837573810955419, -6.172832027328289506, -8.283357778048664244 ) ) ;
#15592 = AXIS2_PLACEMENT_3D ( 'NONE', #7912, #13447, #1028 ) ;
#15593 = DIRECTION ( 'NONE',  ( -0.000000000000000000, -0.000000000000000000, -1.000000000000000000 ) ) ;
#15594 = CARTESIAN_POINT ( 'NONE',  ( -23.02601376483258022, 3.965314980223224151, -6.000000000000000000 ) ) ;
#15595 = EDGE_CURVE ( 'NONE', #7960, #4832, #6035, .T. ) ;
#15596 = CONICAL_SURFACE ( 'NONE', #11211, 3.999999999999986677, 0.7853981633974400633 ) ;
#15597 = ORIENTED_EDGE ( 'NONE', *, *, #9850, .F. ) ;
#15598 = CARTESIAN_POINT ( 'NONE',  ( 29.49337484321020497, -2.602568060005117090, -4.705209693361161349 ) ) ;
#15599 = CARTESIAN_POINT ( 'NONE',  ( -10.27627944162886209, -4.200961894323246071, -11.72793873352920890 ) ) ;
#15600 = CARTESIAN_POINT ( 'NONE',  ( -2.016448651773435938E-27, -20.49999999999999645, -13.00000000000000178 ) ) ;
#15601 = CARTESIAN_POINT ( 'NONE',  ( 26.00079723459025871, -4.771832887959356562, -3.592817407220987747 ) ) ;
#15602 = CARTESIAN_POINT ( 'NONE',  ( 25.93714794488954212, -2.393855775999666591, 5.783357778048667797 ) ) ;
#15603 =( BOUNDED_CURVE ( )  B_SPLINE_CURVE ( 3, ( #17441, #16062, #8626, #12435 ),
 .UNSPECIFIED., .F., .T. ) 
 B_SPLINE_CURVE_WITH_KNOTS ( ( 4, 4 ),
 ( 1.221730476396036824, 1.230954889131919305 ),
 .UNSPECIFIED. ) 
 CURVE ( )  GEOMETRIC_REPRESENTATION_ITEM ( )  RATIONAL_B_SPLINE_CURVE ( ( 1.000000000000000000, 0.9999929091967096895, 0.9999929091967096895, 1.000000000000000000 ) ) 
 REPRESENTATION_ITEM ( '' )  );
#15604 = CARTESIAN_POINT ( 'NONE',  ( 27.21934464581372737, -3.303641803799556964, 3.283357778048666464 ) ) ;
#15605 = PLANE ( 'NONE',  #1375 ) ;
#15606 = VERTEX_POINT ( 'NONE', #4591 ) ;
#15607 = DIRECTION ( 'NONE',  ( -0.1196152422706610735, 0.9928203230275511881, 0.000000000000000000 ) ) ;
#15608 = EDGE_LOOP ( 'NONE', ( #8823, #16680, #9684, #10321 ) ) ;
#15609 = EDGE_CURVE ( 'NONE', #5285, #1869, #15843, .T. ) ;
#15610 = ORIENTED_EDGE ( 'NONE', *, *, #2645, .F. ) ;
#15611 = CARTESIAN_POINT ( 'NONE',  ( -16.75000000000000355, -15.80559819018441381, -16.03574476417185934 ) ) ;
#15612 = VERTEX_POINT ( 'NONE', #349 ) ;
#15613 = CARTESIAN_POINT ( 'NONE',  ( -45.00000000000000711, -16.03270077640482683, -0.5379818257722508434 ) ) ;
#15614 = EDGE_CURVE ( 'NONE', #9143, #1544, #11564, .T. ) ;
#15615 = VECTOR ( 'NONE', #1307, 1000.000000000000000 ) ;
#15616 =( BOUNDED_CURVE ( )  B_SPLINE_CURVE ( 2, ( #16639, #9992, #6837, #1678, #224, #4215, #8473, #5734, #7212 ),
 .UNSPECIFIED., .F., .T. ) 
 B_SPLINE_CURVE_WITH_KNOTS ( ( 3, 2, 2, 2, 3 ),
 ( 0.5576923076923077094, 0.5641025641025640969, 0.5769230769230768718, 0.5897435897435897578, 0.5961538461538461453 ),
 .UNSPECIFIED. ) 
 CURVE ( )  GEOMETRIC_REPRESENTATION_ITEM ( )  RATIONAL_B_SPLINE_CURVE ( ( 0.9330127018922194093, 0.9330127018922194093, 1.000000000000000000, 0.8660254037844387076, 1.000000000000000000, 0.8660254037844387076, 1.000000000000000000, 0.9330127018922194093, 0.9330127018922194093 ) ) 
 REPRESENTATION_ITEM ( '' )  );
#15617 = CARTESIAN_POINT ( 'NONE',  ( 30.02326902268086428, -5.673578940050561847, -3.627061608673667781 ) ) ;
#15618 = CARTESIAN_POINT ( 'NONE',  ( 27.96989853965305528, -4.667028466753395222, -8.283357778048662468 ) ) ;
#15619 = LINE ( 'NONE', #8083, #6364 ) ;
#15620 = FACE_BOUND ( 'NONE', #17224, .T. ) ;
#15621 = CARTESIAN_POINT ( 'NONE',  ( 32.53688598753899441, -6.297517047505613697, -7.033357778048666908 ) ) ;
#15622 = AXIS2_PLACEMENT_3D ( 'NONE', #6244, #10406, #2271 ) ;
#15623 = EDGE_CURVE ( 'NONE', #15456, #558, #3829, .T. ) ;
#15624 = FACE_OUTER_BOUND ( 'NONE', #6919, .T. ) ;
#15625 = VERTEX_POINT ( 'NONE', #17132 ) ;
#15626 = CARTESIAN_POINT ( 'NONE',  ( 26.83664947211162399, -6.984282976826746037, 7.033357778048657138 ) ) ;
#15627 = AXIS2_PLACEMENT_3D ( 'NONE', #4222, #1243, #6932 ) ;
#15628 = AXIS2_PLACEMENT_3D ( 'NONE', #13371, #13722, #12275 ) ;
#15629 = CARTESIAN_POINT ( 'NONE',  ( 30.42903939560917337, -1.852671564043892660, -5.783357778048658027 ) ) ;
#15630 = CARTESIAN_POINT ( 'NONE',  ( -26.79284261260708178, -21.20213040957736794, 14.03697675243215848 ) ) ;
#15631 = DIRECTION ( 'NONE',  ( 0.000000000000000000, -0.5000000000000011102, -0.8660254037844379305 ) ) ;
#15632 = VERTEX_POINT ( 'NONE', #1894 ) ;
#15633 = CARTESIAN_POINT ( 'NONE',  ( 26.31556265977298992, -7.384422263489805793, -5.783357778048663356 ) ) ;
#15634 = ORIENTED_EDGE ( 'NONE', *, *, #6450, .F. ) ;
#15635 = CIRCLE ( 'NONE', #12442, 0.8999999999999998002 ) ;
#15636 = CARTESIAN_POINT ( 'NONE',  ( -1.499999999999999334, 5.809475019311126864, -1.901951201008075243 ) ) ;
#15637 = CARTESIAN_POINT ( 'NONE',  ( 26.39379627684682106, -4.856917663858078882, -3.283357778048664688 ) ) ;
#15638 = ORIENTED_EDGE ( 'NONE', *, *, #13658, .T. ) ;
#15639 = FACE_OUTER_BOUND ( 'NONE', #16109, .T. ) ;
#15640 = CARTESIAN_POINT ( 'NONE',  ( 32.34167700165585302, -2.686501913001913433, -8.283357778048658915 ) ) ;
#15641 = CARTESIAN_POINT ( 'NONE',  ( 26.64639396487419987, -2.308405637095112706, -5.783357778048658027 ) ) ;
#15642 = PRODUCT_CONTEXT ( 'NONE', #10482, 'mechanical' ) ;
#15643 = CYLINDRICAL_SURFACE ( 'NONE', #9246, 10.50000000000000000 ) ;
#15644 = AXIS2_PLACEMENT_3D ( 'NONE', #3045, #12557, #3314 ) ;
#15645 = CARTESIAN_POINT ( 'NONE',  ( 32.06767520579373354, -2.292415704734142690, -6.861505862736158257 ) ) ;
#15646 = EDGE_CURVE ( 'NONE', #131, #11660, #14875, .T. ) ;
#15647 = CARTESIAN_POINT ( 'NONE',  ( 32.87199790123699472, -1.558343308739095656, 5.783357778048663356 ) ) ;
#15648 = CARTESIAN_POINT ( 'NONE',  ( 30.93831368681553684, -6.190304661545915188, 6.861505862736157368 ) ) ;
#15649 = AXIS2_PLACEMENT_3D ( 'NONE', #9341, #6621, #9424 ) ;
#15650 = ORIENTED_EDGE ( 'NONE', *, *, #9344, .T. ) ;
#15651 = LINE ( 'NONE', #7324, #15757 ) ;
#15652 = ORIENTED_EDGE ( 'NONE', *, *, #14911, .F. ) ;
#15653 = ADVANCED_FACE ( 'NONE', ( #15567 ), #252, .F. ) ;
#15654 = CARTESIAN_POINT ( 'NONE',  ( 31.41531425212677675, -1.744041783721344219, 5.783357778048668685 ) ) ;
#15655 = FACE_OUTER_BOUND ( 'NONE', #6864, .T. ) ;
#15656 = CARTESIAN_POINT ( 'NONE',  ( 26.15738093914773543, -4.885401043216321959, -8.283357778048662468 ) ) ;
#15657 = CIRCLE ( 'NONE', #11318, 5.000000000000000888 ) ;
#15658 = VERTEX_POINT ( 'NONE', #5763 ) ;
#15659 = CARTESIAN_POINT ( 'NONE',  ( 0.000000000000000000, 0.000000000000000000, -4.000000000000000000 ) ) ;
#15660 = CARTESIAN_POINT ( 'NONE',  ( -4.000000000000000000, 0.8730390046629853407, -2.923132639555973800 ) ) ;
#15661 = CARTESIAN_POINT ( 'NONE',  ( 3.538288549924106796, -15.34800872113743431, -13.00000000000000178 ) ) ;
#15662 = CARTESIAN_POINT ( 'NONE',  ( 25.90899358965569022, -2.397247819800704782, -6.453230759126464378 ) ) ;
#15663 = AXIS2_PLACEMENT_3D ( 'NONE', #11136, #3101, #9696 ) ;
#15664 = CARTESIAN_POINT ( 'NONE',  ( 26.03726795043090547, -3.446058701420613879, -8.283357778048658915 ) ) ;
#15665 =( GEOMETRIC_REPRESENTATION_CONTEXT ( 3 ) GLOBAL_UNCERTAINTY_ASSIGNED_CONTEXT ( ( #17345 ) ) GLOBAL_UNIT_ASSIGNED_CONTEXT ( ( #1812, #3153, #2983 ) ) REPRESENTATION_CONTEXT ( 'NONE', 'WORKASPACE' ) );
#15666 = CARTESIAN_POINT ( 'NONE',  ( 28.59863824134335530, -19.00380184606325429, 13.55546330914018149 ) ) ;
#15667 = DIRECTION ( 'NONE',  ( -1.000000000000000000, 0.000000000000000000, 0.000000000000000000 ) ) ;
#15668 =( NAMED_UNIT ( * ) PLANE_ANGLE_UNIT ( ) SI_UNIT ( $, .RADIAN. ) );
#15669 = CARTESIAN_POINT ( 'NONE',  ( 31.53813789838894621, -6.745008222462202774, -5.783357778048668685 ) ) ;
#15670 = VERTEX_POINT ( 'NONE', #11277 ) ;
#15671 = EDGE_CURVE ( 'NONE', #16160, #118, #15482, .T. ) ;
#15672 = CIRCLE ( 'NONE', #17141, 2.000000000000001776 ) ;
#15673 = ADVANCED_FACE ( 'NONE', ( #8684 ), #6999, .F. ) ;
#15674 = AXIS2_PLACEMENT_3D ( 'NONE', #10852, #6972, #6876 ) ;
#15675 = CARTESIAN_POINT ( 'NONE',  ( 32.90454166015506132, -1.164874252460851300, 5.783357778048668685 ) ) ;
#15676 = VERTEX_POINT ( 'NONE', #3685 ) ;
#15677 = ORIENTED_EDGE ( 'NONE', *, *, #17640, .F. ) ;
#15678 = VERTEX_POINT ( 'NONE', #13391 ) ;
#15679 = CARTESIAN_POINT ( 'NONE',  ( 30.01874226414561875, -2.539271660970221944, 4.705209693361167567 ) ) ;
#15680 = CARTESIAN_POINT ( 'NONE',  ( 33.30663696749426350, -1.516174747195734085, 5.783357778048668685 ) ) ;
#15681 = DIRECTION ( 'NONE',  ( 0.6000000000000001998, -0.7999999999999999334, 0.000000000000000000 ) ) ;
#15682 = CARTESIAN_POINT ( 'NONE',  ( 26.31556265977298992, -7.384422263489805793, 5.783357778048663356 ) ) ;
#15683 = CARTESIAN_POINT ( 'NONE',  ( -24.42841412577760352, -22.30604244805903136, -14.60923613736931514 ) ) ;
#15684 = CARTESIAN_POINT ( 'NONE',  ( 30.91186687973582536, -2.431667782610909434, -4.705209693361160461 ) ) ;
#15685 = CARTESIAN_POINT ( 'NONE',  ( 31.98525019727866692, -6.363978266284800789, -7.033357778048666908 ) ) ;
#15686 = CARTESIAN_POINT ( 'NONE',  ( 27.27683486999669427, -2.232449958253242883, -5.783357778048658027 ) ) ;
#15687 = AXIS2_PLACEMENT_3D ( 'NONE', #3235, #12568, #16846 ) ;
#15688 = DIRECTION ( 'NONE',  ( 0.000000000000000000, 0.000000000000000000, 1.000000000000000000 ) ) ;
#15689 = CARTESIAN_POINT ( 'NONE',  ( 28.09753128235661279, -6.832371619143005503, -4.533357778048668685 ) ) ;
#15690 = UNCERTAINTY_MEASURE_WITH_UNIT (LENGTH_MEASURE( 1.000000000000000082E-05 ), #14317, 'distance_accuracy_value', 'NONE');
#15691 = CARTESIAN_POINT ( 'NONE',  ( 25.92467471225709374, -2.732717170633701453, -7.033357778048658027 ) ) ;
#15692 = ORIENTED_EDGE ( 'NONE', *, *, #11592, .T. ) ;
#15693 = CONICAL_SURFACE ( 'NONE', #8465, 2.055000000000000160, 0.7853981633974794763 ) ;
#15694 = CARTESIAN_POINT ( 'NONE',  ( 28.34209327568754233, -5.876127416962207306, -7.939653947423664704 ) ) ;
#15695 = CARTESIAN_POINT ( 'NONE',  ( 5.499998817156068753, -20.49639288455253450, -12.00000000000000000 ) ) ;
#15696 = CARTESIAN_POINT ( 'NONE',  ( 32.33415724766913257, -1.960501102408027219, -4.533357778048659803 ) ) ;
#15697 = CARTESIAN_POINT ( 'NONE',  ( 26.13631296615022137, -5.896629108145342357, -3.732065232213778394 ) ) ;
#15698 = DIRECTION ( 'NONE',  ( -1.000000000000000000, 0.000000000000000000, 0.000000000000000000 ) ) ;
#15699 = EDGE_CURVE ( 'NONE', #317, #16897, #7597, .T. ) ;
#15700 = CARTESIAN_POINT ( 'NONE',  ( 27.02423718196931546, -4.780961985016209503, 8.283357778048662468 ) ) ;
#15701 = CARTESIAN_POINT ( 'NONE',  ( 26.45077056032005913, -6.103994453487816330, -7.939653947423662927 ) ) ;
#15702 = CIRCLE ( 'NONE', #16559, 5.500000000000000000 ) ;
#15703 = ORIENTED_EDGE ( 'NONE', *, *, #6215, .T. ) ;
#15704 = EDGE_CURVE ( 'NONE', #4898, #14980, #9878, .T. ) ;
#15705 = CYLINDRICAL_SURFACE ( 'NONE', #15439, 2.500000000000001776 ) ;
#15706 = ORIENTED_EDGE ( 'NONE', *, *, #3300, .F. ) ;
#15707 = VECTOR ( 'NONE', #4226, 1000.000000000000227 ) ;
#15708 = CARTESIAN_POINT ( 'NONE',  ( 23.00000000000000000, -16.21813761408365195, 0.000000000000000000 ) ) ;
#15709 = ORIENTED_EDGE ( 'NONE', *, *, #5828, .T. ) ;
#15710 =( BOUNDED_CURVE ( )  B_SPLINE_CURVE ( 2, ( #8833, #15814, #17197, #7657, #2545, #17287, #4823, #16098, #10353 ),
 .UNSPECIFIED., .F., .T. ) 
 B_SPLINE_CURVE_WITH_KNOTS ( ( 3, 2, 2, 2, 3 ),
 ( 0.7500000000000000000, 0.7564102564102563875, 0.7692307692307692735, 0.7820512820512820484, 0.7884615384615384359 ),
 .UNSPECIFIED. ) 
 CURVE ( )  GEOMETRIC_REPRESENTATION_ITEM ( )  RATIONAL_B_SPLINE_CURVE ( ( 0.9330127018922194093, 0.9330127018922194093, 1.000000000000000000, 0.8660254037844387076, 1.000000000000000000, 0.8660254037844387076, 1.000000000000000000, 0.9330127018922194093, 0.9330127018922194093 ) ) 
 REPRESENTATION_ITEM ( '' )  );
#15711 = CARTESIAN_POINT ( 'NONE',  ( 26.39370705969127684, -2.976016814310973313, -6.861505862736158257 ) ) ;
#15712 = CIRCLE ( 'NONE', #7026, 2.000000000000001776 ) ;
#15713 = CARTESIAN_POINT ( 'NONE',  ( 27.78610916120306129, -6.570083055755264745, -4.705209693361169343 ) ) ;
#15714 = APPLICATION_CONTEXT ( 'automotive_design' ) ;
#15715 = ORIENTED_EDGE ( 'NONE', *, *, #12586, .F. ) ;
#15716 =( BOUNDED_CURVE ( )  B_SPLINE_CURVE ( 3, ( #10249, #11702, #6360, #3373 ),
 .UNSPECIFIED., .F., .T. ) 
 B_SPLINE_CURVE_WITH_KNOTS ( ( 4, 4 ),
 ( 5.052230418047667371, 5.061454830783549852 ),
 .UNSPECIFIED. ) 
 CURVE ( )  GEOMETRIC_REPRESENTATION_ITEM ( )  RATIONAL_B_SPLINE_CURVE ( ( 1.000000000000000000, 0.9999929091967096895, 0.9999929091967096895, 1.000000000000000000 ) ) 
 REPRESENTATION_ITEM ( '' )  );
#15717 = EDGE_LOOP ( 'NONE', ( #1293, #15353, #10874, #13898 ) ) ;
#15718 = CARTESIAN_POINT ( 'NONE',  ( 26.21417678486618641, -2.370676134166772808, -5.783357778048658027 ) ) ;
#15719 = DIRECTION ( 'NONE',  ( -0.8660254037844329345, 0.5000000000000099920, 0.000000000000000000 ) ) ;
#15720 = CARTESIAN_POINT ( 'NONE',  ( 28.45891156537951971, -2.090033060632186412, -5.783357778048670461 ) ) ;
#15721 = CARTESIAN_POINT ( 'NONE',  ( 27.82847066025702887, -2.165988739474055791, 5.783357778048667797 ) ) ;
#15722 = ORIENTED_EDGE ( 'NONE', *, *, #5037, .T. ) ;
#15723 = CARTESIAN_POINT ( 'NONE',  ( 30.17644170758179101, -4.401183590806859947, -3.283357778048664688 ) ) ;
#15724 = EDGE_CURVE ( 'NONE', #2087, #172, #9300, .T. ) ;
#15725 = CARTESIAN_POINT ( 'NONE',  ( 29.23078034989804763, -4.515117109069654688, -8.283357778048662468 ) ) ;
#15726 = CARTESIAN_POINT ( 'NONE',  ( 31.51169109130924184, -2.986371343527201905, 7.939653947423664704 ) ) ;
#15727 = ADVANCED_FACE ( 'NONE', ( #11928, #2167 ), #3508, .T. ) ;
#15728 = CARTESIAN_POINT ( 'NONE',  ( 30.69058026372202974, -5.793053633118939061, -8.283357778048664244 ) ) ;
#15729 = CARTESIAN_POINT ( 'NONE',  ( 29.82675284572052732, -1.925235199084722959, -5.113484796970855228 ) ) ;
#15730 = DIRECTION ( 'NONE',  ( -1.000000000000000000, 0.000000000000000000, 0.000000000000000000 ) ) ;
#15731 = ORIENTED_EDGE ( 'NONE', *, *, #1311, .T. ) ;
#15732 = DIRECTION ( 'NONE',  ( 1.000000000000000000, 0.000000000000000000, 0.000000000000000000 ) ) ;
#15733 = ORIENTED_EDGE ( 'NONE', *, *, #6595, .T. ) ;
#15734 = CYLINDRICAL_SURFACE ( 'NONE', #2335, 2.749999999999992006 ) ;
#15735 =( BOUNDED_CURVE ( )  B_SPLINE_CURVE ( 2, ( #6924, #15183, #11077, #5463, #45, #14092, #132, #5645, #2845 ),
 .UNSPECIFIED., .F., .T. ) 
 B_SPLINE_CURVE_WITH_KNOTS ( ( 3, 2, 2, 2, 3 ),
 ( 0.3269230769230769273, 0.3333333333333333148, 0.3461538461538461453, 0.3589743589743589758, 0.3653846153846154188 ),
 .UNSPECIFIED. ) 
 CURVE ( )  GEOMETRIC_REPRESENTATION_ITEM ( )  RATIONAL_B_SPLINE_CURVE ( ( 0.9330127018922194093, 0.9330127018922194093, 1.000000000000000000, 0.8660254037844387076, 1.000000000000000000, 0.8660254037844387076, 1.000000000000000000, 0.9330127018922190762, 0.9330127018922194093 ) ) 
 REPRESENTATION_ITEM ( '' )  );
#15736 = CARTESIAN_POINT ( 'NONE',  ( 25.07353123778398896, 1.235291682954687165, 14.60266621045498425 ) ) ;
#15737 = DIRECTION ( 'NONE',  ( -0.05980762113533042573, 0.4964101615137759271, -0.8660254037844383745 ) ) ;
#15738 = CARTESIAN_POINT ( 'NONE',  ( 31.98525019727866692, -6.363978266284800789, -7.033357778048666908 ) ) ;
#15739 = AXIS2_PLACEMENT_3D ( 'NONE', #3337, #10117, #12858 ) ;
#15740 = LINE ( 'NONE', #5652, #13039 ) ;
#15741 = DIRECTION ( 'NONE',  ( 0.9928203230275510771, 0.1196152422706614621, -0.000000000000000000 ) ) ;
#15742 = DIRECTION ( 'NONE',  ( -1.000000000000000000, 0.000000000000000000, 0.000000000000000000 ) ) ;
#15743 = EDGE_CURVE ( 'NONE', #16997, #627, #6559, .T. ) ;
#15744 = CARTESIAN_POINT ( 'NONE',  ( 26.01652455409633902, -4.902371455920926380, 5.783357778048663356 ) ) ;
#15745 = CARTESIAN_POINT ( 'NONE',  ( 31.43732351782677625, -4.249272233123119413, -3.283357778048664688 ) ) ;
#15746 = AXIS2_PLACEMENT_3D ( 'NONE', #474, #10155, #7101 ) ;
#15747 = CARTESIAN_POINT ( 'NONE',  ( 28.89355063163679915, -2.047864499088824175, 5.783357778048668685 ) ) ;
#15748 = EDGE_LOOP ( 'NONE', ( #17107, #10336 ) ) ;
#15749 = CARTESIAN_POINT ( 'NONE',  ( 33.68284756902015431, -1.652629194728085338, -9.783357778048662468 ) ) ;
#15750 = ORIENTED_EDGE ( 'NONE', *, *, #10374, .T. ) ;
#15751 = CARTESIAN_POINT ( 'NONE',  ( 32.29974222271236073, -2.891426744974864071, 7.939653947423664704 ) ) ;
#15752 = FACE_OUTER_BOUND ( 'NONE', #15333, .T. ) ;
#15753 = CYLINDRICAL_SURFACE ( 'NONE', #2112, 6.249999999999998224 ) ;
#15754 = ORIENTED_EDGE ( 'NONE', *, *, #9883, .T. ) ;
#15755 = CARTESIAN_POINT ( 'NONE',  ( 25.90934487712387480, 0.1208734971681818676, 4.216642221951339309 ) ) ;
#15756 = CARTESIAN_POINT ( 'NONE',  ( 26.01652455409633902, -4.902371455920926380, -5.783357778048663356 ) ) ;
#15757 = VECTOR ( 'NONE', #7412, 1000.000000000000114 ) ;
#15758 = EDGE_CURVE ( 'NONE', #15540, #11613, #1829, .T. ) ;
#15759 = DIRECTION ( 'NONE',  ( 0.000000000000000000, 0.000000000000000000, -1.000000000000000000 ) ) ;
#15760 = CARTESIAN_POINT ( 'NONE',  ( 27.48088551392658729, -7.244023872874614689, -5.783357778048657138 ) ) ;
#15761 = CARTESIAN_POINT ( 'NONE',  ( 26.87785582392756467, -3.344784462964796479, -3.283357778048662023 ) ) ;
#15762 = CARTESIAN_POINT ( 'NONE',  ( -2.016448651773435938E-27, -20.49999999999999645, -12.00000000000000000 ) ) ;
#15763 = FACE_OUTER_BOUND ( 'NONE', #15109, .T. ) ;
#15764 = APPLICATION_PROTOCOL_DEFINITION ( 'draft international standard', 'automotive_design', 1998, #17356 ) ;
#15765 = CARTESIAN_POINT ( 'NONE',  ( 28.77978050244509944, -3.315512618508630993, -7.939653947423660263 ) ) ;
#15766 = CARTESIAN_POINT ( 'NONE',  ( 25.79194807336802953, -3.038360733637177624, -6.974889548725401234 ) ) ;
#15767 = CARTESIAN_POINT ( 'NONE',  ( 32.30788887834420819, -1.963665922152317833, 4.533357778048667797 ) ) ;
#15768 = ORIENTED_EDGE ( 'NONE', *, *, #2717, .T. ) ;
#15769 = VERTEX_POINT ( 'NONE', #17515 ) ;
#15770 = ORIENTED_EDGE ( 'NONE', *, *, #3743, .F. ) ;
#15771 = CARTESIAN_POINT ( 'NONE',  ( 25.99795558426325215, -4.648046406214923820, 7.939653947423662039 ) ) ;
#15772 = CARTESIAN_POINT ( 'NONE',  ( 32.18597209352066812, -4.159074864394664672, 3.627061608673664228 ) ) ;
#15773 = CARTESIAN_POINT ( 'NONE',  ( 27.17934203385504333, -30.00000000000000355, -13.93658524716016878 ) ) ;
#15774 = DIRECTION ( 'NONE',  ( 0.9928203230275510771, 0.1196152422706609902, 4.006172263299092517E-17 ) ) ;
#15775 = EDGE_CURVE ( 'NONE', #3948, #10789, #3268, .T. ) ;
#15776 = FACE_BOUND ( 'NONE', #11396, .T. ) ;
#15777 = CARTESIAN_POINT ( 'NONE',  ( 25.60565592828815440, -3.070961412863312034, -6.861505862736159145 ) ) ;
#15778 = CARTESIAN_POINT ( 'NONE',  ( -8.661840944284252430E-17, -4.736529461165884136, -3.381130640444275581 ) ) ;
#15779 = DIRECTION ( 'NONE',  ( 0.1414213562373112243, -0.9899494936611663576, 0.000000000000000000 ) ) ;
#15780 = CARTESIAN_POINT ( 'NONE',  ( 29.42285898892238549, -7.010054420087358018, -5.113484796970856117 ) ) ;
#15781 = CARTESIAN_POINT ( 'NONE',  ( 26.67454832010805532, -2.305013593294074514, -5.113484796970851676 ) ) ;
#15782 = DIRECTION ( 'NONE',  ( 0.9928203230275512992, 0.1196152422706610180, 4.006172263299093133E-17 ) ) ;
#15783 = VERTEX_POINT ( 'NONE', #14758 ) ;
#15784 = CARTESIAN_POINT ( 'NONE',  ( 27.10313151398701947, -6.652368374500619908, -6.861505862736166250 ) ) ;
#15785 = EDGE_CURVE ( 'NONE', #7830, #17725, #16583, .T. ) ;
#15786 = PLANE ( 'NONE',  #7561 ) ;
#15787 = EDGE_LOOP ( 'NONE', ( #912, #9846, #1566, #9991 ) ) ;
#15788 = CARTESIAN_POINT ( 'NONE',  ( -10.37836969302994028, 0.6704047395399693743, -6.899999999999998579 ) ) ;
#15789 = PRODUCT_DEFINITION ( 'UNKNOWN', '', #5696, #15872 ) ;
#15790 = CARTESIAN_POINT ( 'NONE',  ( 27.84978555093622177, -3.227686124957687586, 3.283357778048666464 ) ) ;
#15791 = VERTEX_POINT ( 'NONE', #5118 ) ;
#15792 = LINE ( 'NONE', #2634, #12377 ) ;
#15793 = CARTESIAN_POINT ( 'NONE',  ( 31.08270050955629671, -4.291997302367946077, -3.627061608673664672 ) ) ;
#15794 = ORIENTED_EDGE ( 'NONE', *, *, #12326, .T. ) ;
#15795 = ADVANCED_FACE ( 'NONE', ( #10639, #2424 ), #5038, .F. ) ;
#15796 = FACE_OUTER_BOUND ( 'NONE', #13906, .T. ) ;
#15797 = CARTESIAN_POINT ( 'NONE',  ( 33.48996557372703364, -1.821249024531260696, -7.033357778048658027 ) ) ;
#15798 = EDGE_CURVE ( 'NONE', #4809, #15874, #16137, .T. ) ;
#15799 = ORIENTED_EDGE ( 'NONE', *, *, #218, .F. ) ;
#15800 = CARTESIAN_POINT ( 'NONE',  ( 27.65458886993626564, -2.824105456627233224, -6.861505862736158257 ) ) ;
#15801 = CARTESIAN_POINT ( 'NONE',  ( 26.55511561737958814, -2.656761491791831187, -7.033357778048658027 ) ) ;
#15802 = CARTESIAN_POINT ( 'NONE',  ( 26.24062359194589078, -6.129313013101781671, -3.627061608673667781 ) ) ;
#15803 = EDGE_CURVE ( 'NONE', #5445, #10572, #6314, .T. ) ;
#15804 = CARTESIAN_POINT ( 'NONE',  ( 26.01652455409633902, -4.902371455920926380, -5.783357778048663356 ) ) ;
#15805 = DIRECTION ( 'NONE',  ( 0.1113444980252557837, 0.9937818688019538493, 0.000000000000000000 ) ) ;
#15806 = CARTESIAN_POINT ( 'NONE',  ( 0.000000000000000000, 0.000000000000000000, 0.000000000000000000 ) ) ;
#15807 = CARTESIAN_POINT ( 'NONE',  ( 27.45957062324739795, -6.182326487390973568, -8.283357778048662468 ) ) ;
#15808 = DIRECTION ( 'NONE',  ( -0.8191520442889900222, 0.000000000000000000, -0.5735764363510486019 ) ) ;
#15809 = CARTESIAN_POINT ( 'NONE',  ( 30.75425665345519732, -2.450656702321377001, 6.861505862736165362 ) ) ;
#15810 =( BOUNDED_CURVE ( )  B_SPLINE_CURVE ( 2, ( #16400, #5577, #65, #4233, #2609, #8138, #9732, #13834, #8224 ),
 .UNSPECIFIED., .F., .T. ) 
 B_SPLINE_CURVE_WITH_KNOTS ( ( 3, 2, 2, 2, 3 ),
 ( 0.7500000000000000000, 0.7564102564102563875, 0.7692307692307692735, 0.7820512820512820484, 0.7884615384615384359 ),
 .UNSPECIFIED. ) 
 CURVE ( )  GEOMETRIC_REPRESENTATION_ITEM ( )  RATIONAL_B_SPLINE_CURVE ( ( 0.9330127018922194093, 0.9330127018922194093, 1.000000000000000000, 0.8660254037844387076, 1.000000000000000000, 0.8660254037844387076, 1.000000000000000000, 0.9330127018922194093, 0.9330127018922194093 ) ) 
 REPRESENTATION_ITEM ( '' )  );
#15811 = EDGE_LOOP ( 'NONE', ( #12008, #9121, #14313, #11521 ) ) ;
#15812 = DIRECTION ( 'NONE',  ( -1.000000000000000000, -0.000000000000000000, -0.000000000000000000 ) ) ;
#15813 = CARTESIAN_POINT ( 'NONE',  ( 8.409399735147211686E-16, 4.618802153517009401, -3.133295621305383083 ) ) ;
#15814 = CARTESIAN_POINT ( 'NONE',  ( 28.08317206381523334, -7.171460237833785278, 6.453230759126462601 ) ) ;
#15815 = ORIENTED_EDGE ( 'NONE', *, *, #6425, .F. ) ;
#15816 = DIRECTION ( 'NONE',  ( 0.9928203230275512992, 0.1196152422706587698, 0.000000000000000000 ) ) ;
#15817 = CARTESIAN_POINT ( 'NONE',  ( 0.000000000000000000, 1.178949249685213863, -2.042000000000001148 ) ) ;
#15818 = EDGE_CURVE ( 'NONE', #12534, #692, #5205, .T. ) ;
#15819 = CARTESIAN_POINT ( 'NONE',  ( 26.75784435724945709, -6.993777436889428323, -4.533357778048668685 ) ) ;
#15820 = DIRECTION ( 'NONE',  ( -0.6047431568147647596, -0.4535573676110720709, 0.6546536707079764206 ) ) ;
#15821 = ORIENTED_EDGE ( 'NONE', *, *, #2994, .T. ) ;
#15822 = CARTESIAN_POINT ( 'NONE',  ( 30.41656616297672500, -2.191532958677927745, -7.033357778048658027 ) ) ;
#15823 = CARTESIAN_POINT ( 'NONE',  ( -35.62429925076629189, -17.76690233603958546, 10.53798182577225084 ) ) ;
#15824 = ITEM_DEFINED_TRANSFORMATION ( 'NONE', 'NONE', #1620,  #3575 ) ;
#15825 = CARTESIAN_POINT ( 'NONE',  ( -8.632250723006722026, -18.84644399697197770, -16.84735068286508763 ) ) ;
#15826 = ADVANCED_FACE ( 'NONE', ( #16038 ), #3609, .F. ) ;
#15827 = CARTESIAN_POINT ( 'NONE',  ( 30.30787278169304244, -6.266260340387784566, -4.705209693361169343 ) ) ;
#15828 = CARTESIAN_POINT ( 'NONE',  ( 42.73333828282231650, -6.338146013849483396, -5.783357778048662468 ) ) ;
#15829 = CARTESIAN_POINT ( 'NONE',  ( 31.00882954110335632, -1.782818301463667598, -5.113484796970851676 ) ) ;
#15830 = CARTESIAN_POINT ( 'NONE',  ( 27.26074174026764751, -6.633379454790151009, 4.705209693361159573 ) ) ;
#15831 = ORIENTED_EDGE ( 'NONE', *, *, #17819, .T. ) ;
#15832 = B_SPLINE_CURVE_WITH_KNOTS ( 'NONE', 1,
 ( #13599, #5153 ),
 .UNSPECIFIED., .F., .F.,
 ( 2, 2 ),
 ( 0.000000000000000000, 1.000000000000000000 ),
 .UNSPECIFIED. ) ;
#15833 = CARTESIAN_POINT ( 'NONE',  ( 26.25801688195511474, -3.619335333876111171, -7.939653947423660263 ) ) ;
#15834 =( BOUNDED_CURVE ( )  B_SPLINE_CURVE ( 3, ( #7980, #10850, #1008, #9416 ),
 .UNSPECIFIED., .F., .T. ) 
 B_SPLINE_CURVE_WITH_KNOTS ( ( 4, 4 ),
 ( 4.363323129985829496, 4.457746946181837977 ),
 .UNSPECIFIED. ) 
 CURVE ( )  GEOMETRIC_REPRESENTATION_ITEM ( )  RATIONAL_B_SPLINE_CURVE ( ( 1.000000000000000000, 0.9992571499088201969, 0.9992571499088201969, 1.000000000000000000 ) ) 
 REPRESENTATION_ITEM ( '' )  );
#15835 = ORIENTED_EDGE ( 'NONE', *, *, #17477, .F. ) ;
#15836 = CARTESIAN_POINT ( 'NONE',  ( 33.58707084003705745, -6.498152266226123963, 5.783357778048657138 ) ) ;
#15837 = CARTESIAN_POINT ( 'NONE',  ( -25.20502126318114833, -10.36657009486825842, 14.42817146764052083 ) ) ;
#15838 = CARTESIAN_POINT ( 'NONE',  ( 50.00000000000000000, -19.03270077640483038, -5.537981825772250843 ) ) ;
#15839 = ORIENTED_EDGE ( 'NONE', *, *, #6, .T. ) ;
#15840 = CARTESIAN_POINT ( 'NONE',  ( 28.28511899221430070, -4.629050627332469858, -3.283357778048664688 ) ) ;
#15841 = PLANE ( 'NONE',  #15343 ) ;
#15842 = ADVANCED_FACE ( 'NONE', ( #7767 ), #13296, .T. ) ;
#15843 = LINE ( 'NONE', #16855, #9579 ) ;
#15844 = CARTESIAN_POINT ( 'NONE',  ( 32.93018312783485158, -2.815471066132994249, -3.627061608673662008 ) ) ;
#15845 = CARTESIAN_POINT ( 'NONE',  ( 25.40682704530840397, -3.522014380262483702, -8.283357778048658915 ) ) ;
#15846 = CARTESIAN_POINT ( 'NONE',  ( 0.1404055950190656876, 4.699865361596996749, -3.386887224136968300 ) ) ;
#15847 = DIRECTION ( 'NONE',  ( 0.9928203230275510771, 0.1196152422706609902, 4.006172263299092517E-17 ) ) ;
#15848 = ADVANCED_FACE ( 'NONE', ( #10989 ), #12553, .F. ) ;
#15849 = CARTESIAN_POINT ( 'NONE',  ( 27.71165237056504438, -5.952083095804076684, -7.939653947423664704 ) ) ;
#15850 = ORIENTED_EDGE ( 'NONE', *, *, #17551, .T. ) ;
#15851 =( BOUNDED_CURVE ( )  B_SPLINE_CURVE ( 2, ( #15760, #5946, #15390, #7239, #11279, #521, #11566, #2978, #7151 ),
 .UNSPECIFIED., .F., .T. ) 
 B_SPLINE_CURVE_WITH_KNOTS ( ( 3, 2, 2, 2, 3 ),
 ( 0.8269230769230769829, 0.8333333333333333703, 0.8461538461538461453, 0.8589743589743589203, 0.8653846153846154188 ),
 .UNSPECIFIED. ) 
 CURVE ( )  GEOMETRIC_REPRESENTATION_ITEM ( )  RATIONAL_B_SPLINE_CURVE ( ( 0.9330127018922192983, 0.9330127018922198534, 1.000000000000000000, 0.8660254037844387076, 1.000000000000000000, 0.8660254037844387076, 1.000000000000000000, 0.9330127018922187432, 0.9330127018922192983 ) ) 
 REPRESENTATION_ITEM ( '' )  );
#15852 = AXIS2_PLACEMENT_3D ( 'NONE', #17497, #6298, #9365 ) ;
#15853 = CARTESIAN_POINT ( 'NONE',  ( 32.52441275490655670, -6.636378442139655220, -5.783357778048663356 ) ) ;
#15854 = CARTESIAN_POINT ( 'NONE',  ( 32.64947922571280259, -7.010858578292532783, 5.783357778048657138 ) ) ;
#15855 = EDGE_CURVE ( 'NONE', #6589, #9029, #15949, .T. ) ;
#15856 = VERTEX_POINT ( 'NONE', #13738 ) ;
#15857 = AXIS2_PLACEMENT_3D ( 'NONE', #16889, #1291, #15237 ) ;
#15858 = PRODUCT_DEFINITION_FORMATION_WITH_SPECIFIED_SOURCE ( 'ANY', '', #9104, .NOT_KNOWN. ) ;
#15859 = ORIENTED_EDGE ( 'NONE', *, *, #10085, .F. ) ;
#15860 = ORIENTED_EDGE ( 'NONE', *, *, #1481, .F. ) ;
#15861 = CARTESIAN_POINT ( 'NONE',  ( 26.79905070906539777, -3.354278923027479209, 8.283357778048666020 ) ) ;
#15862 = DIRECTION ( 'NONE',  ( 0.000000000000000000, 0.000000000000000000, 1.000000000000000000 ) ) ;
#15863 = CARTESIAN_POINT ( 'NONE',  ( 5.000000000000004441, 0.000000000000000000, 4.250000000000000000 ) ) ;
#15864 = VECTOR ( 'NONE', #7290, 1000.000000000000000 ) ;
#15865 = DIRECTION ( 'NONE',  ( -1.000000000000000000, 0.000000000000000000, 0.000000000000000000 ) ) ;
#15866 = CARTESIAN_POINT ( 'NONE',  ( -26.79284261260708178, -21.20213040957736794, -14.03697675243215848 ) ) ;
#15867 = CARTESIAN_POINT ( 'NONE',  ( 32.18597209352066812, -4.159074864394664672, -7.939653947423662039 ) ) ;
#15868 = CARTESIAN_POINT ( 'NONE',  ( 31.04700706809921940, -2.115577279836057922, -7.033357778048658027 ) ) ;
#15869 = FACE_OUTER_BOUND ( 'NONE', #3237, .T. ) ;
#15870 = DIRECTION ( 'NONE',  ( -1.000000000000000000, -0.000000000000000000, -0.000000000000000000 ) ) ;
#15871 = LINE ( 'NONE', #17541, #940 ) ;
#15872 = PRODUCT_DEFINITION_CONTEXT ( 'detailed design', #2977, 'design' ) ;
#15873 = DIRECTION ( 'NONE',  ( 0.9928203230275510771, 0.1196152422706609902, 4.006172263299092517E-17 ) ) ;
#15874 = VERTEX_POINT ( 'NONE', #11079 ) ;
#15875 = CARTESIAN_POINT ( 'NONE',  ( 33.76207435632690590, -3.969185667289998332, -3.627061608673664672 ) ) ;
#15876 = CARTESIAN_POINT ( 'NONE',  ( 32.95662993491456660, -6.574107945067995118, -5.783357778048669573 ) ) ;
#15877 = ORIENTED_EDGE ( 'NONE', *, *, #9266, .F. ) ;
#15878 = AXIS2_PLACEMENT_3D ( 'NONE', #12871, #11485, #5781 ) ;
#15879 = EDGE_CURVE ( 'NONE', #12766, #1421, #10814, .T. ) ;
#15880 = CARTESIAN_POINT ( 'NONE',  ( 27.29063000668916672, -2.568146533142987575, 7.033357778048666020 ) ) ;
#15881 = EDGE_LOOP ( 'NONE', ( #7611, #10808, #3545, #1355 ) ) ;
#15882 = CARTESIAN_POINT ( 'NONE',  ( 3.999999999999998224, 1.941961291383482280, -0.3515519931180262625 ) ) ;
#15883 = AXIS2_PLACEMENT_3D ( 'NONE', #3454, #4713, #10147 ) ;
#15884 = CARTESIAN_POINT ( 'NONE',  ( 30.75425665345519732, -2.450656702321377001, -4.705209693361161349 ) ) ;
#15885 = ORIENTED_EDGE ( 'NONE', *, *, #14794, .F. ) ;
#15886 = ADVANCED_FACE ( 'NONE', ( #6929 ), #10201, .T. ) ;
#15887 = CARTESIAN_POINT ( 'NONE',  ( 29.77118727536321074, -5.903822331637461396, -3.283357778048667797 ) ) ;
#15888 = DIRECTION ( 'NONE',  ( 0.6047431568147660919, 0.4535573676110685737, 0.6546536707079775308 ) ) ;
#15889 = DIRECTION ( 'NONE',  ( 4.179998415399335043E-17, -3.469446951953615175E-16, 1.000000000000000000 ) ) ;
#15890 = AXIS2_PLACEMENT_3D ( 'NONE', #8398, #4324, #11098 ) ;
#15891 = FACE_OUTER_BOUND ( 'NONE', #14774, .T. ) ;
#15892 = VECTOR ( 'NONE', #12738, 1000.000000000000000 ) ;
#15893 = CARTESIAN_POINT ( 'NONE',  ( 28.41655006632555569, -6.494127376913395366, -4.705209693361169343 ) ) ;
#15894 = CARTESIAN_POINT ( 'NONE',  ( 26.25801688195511474, -3.619335333876111171, -7.939653947423660263 ) ) ;
#15895 = CARTESIAN_POINT ( 'NONE',  ( 35.74085044863416982, 7.999999999999934275, -11.27079897466147429 ) ) ;
#15896 = DIRECTION ( 'NONE',  ( 0.8660254037844328234, -0.5000000000000099920, 0.000000000000000000 ) ) ;
#15897 = CARTESIAN_POINT ( 'NONE',  ( 16.03720890403358013, 12.19600435288735341, -16.13737481314213440 ) ) ;
#15898 = CARTESIAN_POINT ( 'NONE',  ( 27.02423718196931546, -4.780961985016209503, -3.283357778048664688 ) ) ;
#15899 = ADVANCED_FACE ( 'NONE', ( #16643 ), #9718, .T. ) ;
#15900 = LINE ( 'NONE', #5997, #5989 ) ;
#15901 = EDGE_CURVE ( 'NONE', #3432, #3677, #1503, .T. ) ;
#15902 = VECTOR ( 'NONE', #17005, 1000.000000000000000 ) ;
#15903 = EDGE_LOOP ( 'NONE', ( #5801, #12841, #6772, #7954 ) ) ;
#15904 = DIRECTION ( 'NONE',  ( -0.000000000000000000, -0.000000000000000000, -1.000000000000000000 ) ) ;
#15905 = CARTESIAN_POINT ( 'NONE',  ( 30.68374079916737429, -6.858143062403621926, -5.113484796970860558 ) ) ;
#15906 = CARTESIAN_POINT ( 'NONE',  ( 31.61111609099199171, -1.710254666422835745, 5.783357778048665132 ) ) ;
#15907 = ORIENTED_EDGE ( 'NONE', *, *, #7022, .T. ) ;
#15908 = CYLINDRICAL_SURFACE ( 'NONE', #10199, 2.000000000000001776 ) ;
#15909 = FACE_OUTER_BOUND ( 'NONE', #10830, .T. ) ;
#15910 = CARTESIAN_POINT ( 'NONE',  ( 25.85239768453567066, -3.540099486550932983, -4.114102314938801186 ) ) ;
#15911 = CARTESIAN_POINT ( 'NONE',  ( 32.06767520579373354, -2.292415704734142690, -6.861505862736158257 ) ) ;
#15912 = CARTESIAN_POINT ( 'NONE',  ( 34.91600907648203389, -11.88801210197604341, 0.000000000000000000 ) ) ;
#15913 = ORIENTED_EDGE ( 'NONE', *, *, #14410, .T. ) ;
#15914 = VECTOR ( 'NONE', #1167, 1000.000000000000227 ) ;
#15915 = CARTESIAN_POINT ( 'NONE',  ( 28.36392410707646761, -4.619556167269785796, -3.283357778048664688 ) ) ;
#15916 = DIRECTION ( 'NONE',  ( 0.000000000000000000, 0.000000000000000000, 1.000000000000000000 ) ) ;
#15917 = CARTESIAN_POINT ( 'NONE',  ( 1.500000000000000000, 10.39230484541326227, -3.000000000000000000 ) ) ;
#15918 = CARTESIAN_POINT ( 'NONE',  ( 31.67382807612511542, -6.101689702897060030, -6.861505862736167138 ) ) ;
#15919 = DIRECTION ( 'NONE',  ( -0.000000000000000000, 1.000000000000000000, -3.469446951953614189E-16 ) ) ;
#15920 = CARTESIAN_POINT ( 'NONE',  ( 19.43845002722867221, 2.988003976273734263, -6.000000000000000000 ) ) ;
#15921 = CARTESIAN_POINT ( 'NONE',  ( 27.89118264539014547, -6.557423775948280742, 4.705209693361159573 ) ) ;
#15922 = AXIS2_PLACEMENT_3D ( 'NONE', #17862, #16468, #14927 ) ;
#15923 = AXIS2_PLACEMENT_3D ( 'NONE', #4204, #11145, #9704 ) ;
#15924 =( BOUNDED_CURVE ( )  B_SPLINE_CURVE ( 3, ( #2092, #13139, #14688, #15773 ),
 .UNSPECIFIED., .F., .T. ) 
 B_SPLINE_CURVE_WITH_KNOTS ( ( 4, 4 ),
 ( 4.846194975958193929, 4.967031014587541371 ),
 .UNSPECIFIED. ) 
 CURVE ( )  GEOMETRIC_REPRESENTATION_ITEM ( )  RATIONAL_B_SPLINE_CURVE ( ( 1.000000000000000000, 0.9987835910734579326, 0.9987835910734579326, 1.000000000000000000 ) ) 
 REPRESENTATION_ITEM ( '' )  );
#15925 = ADVANCED_FACE ( 'NONE', ( #9464 ), #15003, .F. ) ;
#15926 = VERTEX_POINT ( 'NONE', #12195 ) ;
#15927 = AXIS2_PLACEMENT_3D ( 'NONE', #14921, #10894, #9463 ) ;
#15928 = CARTESIAN_POINT ( 'NONE',  ( 25.60565592828815440, -3.070961412863312034, -6.861505862736159145 ) ) ;
#15929 = ORIENTED_EDGE ( 'NONE', *, *, #13003, .T. ) ;
#15930 = CARTESIAN_POINT ( 'NONE',  ( 25.81100034576892455, -6.186289477007987259, 4.026422103237231376 ) ) ;
#15931 = CARTESIAN_POINT ( 'NONE',  ( -21.03265992632394799, -10.27181489424398997, 15.32141966295701430 ) ) ;
#15932 = CARTESIAN_POINT ( 'NONE',  ( 27.33945763453056088, -4.742984145595265488, -8.283357778048662468 ) ) ;
#15933 = ADVANCED_FACE ( 'NONE', ( #12290 ), #12244, .T. ) ;
#15934 = ORIENTED_EDGE ( 'NONE', *, *, #2656, .F. ) ;
#15935 = ORIENTED_EDGE ( 'NONE', *, *, #7020, .T. ) ;
#15936 = DIRECTION ( 'NONE',  ( -1.000000000000000000, -0.000000000000000000, -0.000000000000000000 ) ) ;
#15937 = ORIENTED_EDGE ( 'NONE', *, *, #4914, .T. ) ;
#15938 = DIRECTION ( 'NONE',  ( -0.000000000000000000, -0.000000000000000000, 1.000000000000000000 ) ) ;
#15939 = CARTESIAN_POINT ( 'NONE',  ( 2.500000000000000000, -2.357898499370431722, 2.818925648462311528E-15 ) ) ;
#15940 = CARTESIAN_POINT ( 'NONE',  ( 31.51169109130924184, -2.986371343527201905, -3.627061608673662896 ) ) ;
#15941 = CARTESIAN_POINT ( 'NONE',  ( 4.197393957002304887, 0.8151795401431362054, -3.203767560748937537 ) ) ;
#15942 = DIRECTION ( 'NONE',  ( -0.1035898384862230376, 0.8598076211353316012, 0.5000000000000004441 ) ) ;
#15943 = APPLICATION_PROTOCOL_DEFINITION ( 'draft international standard', 'automotive_design', 1998, #10482 ) ;
#15944 = CARTESIAN_POINT ( 'NONE',  ( 28.13194630731337753, -5.901445976576171759, -3.627061608673667781 ) ) ;
#15945 = CIRCLE ( 'NONE', #1746, 3.199999999999999289 ) ;
#15946 = CARTESIAN_POINT ( 'NONE',  ( 26.02974819644417792, -2.720057890826728109, -4.533357778048659803 ) ) ;
#15947 = CARTESIAN_POINT ( 'NONE',  ( 31.32102116884452414, -5.717097954277069682, 3.283357778048663800 ) ) ;
#15948 = EDGE_CURVE ( 'NONE', #2020, #13298, #9065, .T. ) ;
#15949 =( BOUNDED_CURVE ( )  B_SPLINE_CURVE ( 2, ( #2771, #13819, #8378, #49, #3949, #5560, #9379, #1406, #1140 ),
 .UNSPECIFIED., .F., .T. ) 
 B_SPLINE_CURVE_WITH_KNOTS ( ( 3, 2, 2, 2, 3 ),
 ( 0.05769230769230771633, 0.06410256410256409687, 0.07692307692307692735, 0.08974358974358974395, 0.09615384615384617306 ),
 .UNSPECIFIED. ) 
 CURVE ( )  GEOMETRIC_REPRESENTATION_ITEM ( )  RATIONAL_B_SPLINE_CURVE ( ( 0.9330127018922194093, 0.9330127018922196314, 1.000000000000000000, 0.8660254037844387076, 1.000000000000000000, 0.8660254037844387076, 1.000000000000000000, 0.9330127018922191873, 0.9330127018922194093 ) ) 
 REPRESENTATION_ITEM ( '' )  );
#15950 = VECTOR ( 'NONE', #9009, 1000.000000000000000 ) ;
#15951 = ORIENTED_EDGE ( 'NONE', *, *, #14226, .F. ) ;
#15952 = AXIS2_PLACEMENT_3D ( 'NONE', #7268, #11497, #12785 ) ;
#15953 = VERTEX_POINT ( 'NONE', #11160 ) ;
#15954 = EDGE_LOOP ( 'NONE', ( #1114, #8862 ) ) ;
#15955 = DIRECTION ( 'NONE',  ( 0.9928203230275512992, 0.1196152422706614898, -0.000000000000000000 ) ) ;
#15956 = PLANE ( 'NONE',  #10778 ) ;
#15957 = EDGE_CURVE ( 'NONE', #1544, #4537, #5380, .T. ) ;
#15958 = FILL_AREA_STYLE ('',( #7787 ) ) ;
#15959 = CLOSED_SHELL ( 'NONE', ( #709, #7219, #5953, #2788, #17361, #2623, #629, #1743, #7242, #15280, #12717, #3984, #16979, #17014, #1538, #12972, #6509 ) ) ;
#15960 = DIRECTION ( 'NONE',  ( 0.000000000000000000, 0.000000000000000000, 1.000000000000000000 ) ) ;
#15961 = STYLED_ITEM ( 'NONE', ( #2530 ), #7664 ) ;
#15962 = CARTESIAN_POINT ( 'NONE',  ( -20.27016866188220945, -21.85533094420792466, -15.46350303853101593 ) ) ;
#15963 = CARTESIAN_POINT ( 'NONE',  ( 30.40841950734487753, -3.119293781500474427, -3.627061608673662008 ) ) ;
#15964 = CYLINDRICAL_SURFACE ( 'NONE', #11897, 6.249999999999998224 ) ;
#15965 = DIRECTION ( 'NONE',  ( -1.000000000000000000, 0.000000000000000000, 0.000000000000000000 ) ) ;
#15966 = CARTESIAN_POINT ( 'NONE',  ( 9.700633612364448766, 16.10095840566074799, 16.79370834700961979 ) ) ;
#15967 = CARTESIAN_POINT ( 'NONE',  ( 31.04700706809921940, -2.115577279836057922, -7.033357778048658027 ) ) ;
#15968 = CIRCLE ( 'NONE', #7559, 13.00000000000000178 ) ;
#15969 = CARTESIAN_POINT ( 'NONE',  ( 0.000000000000000000, 0.000000000000000000, 1.599999999999998979 ) ) ;
#15970 =( NAMED_UNIT ( * ) SI_UNIT ( $, .STERADIAN. ) SOLID_ANGLE_UNIT ( ) );
#15971 = ORIENTED_EDGE ( 'NONE', *, *, #6043, .F. ) ;
#15972 = VECTOR ( 'NONE', #9333, 1000.000000000000114 ) ;
#15973 = ORIENTED_EDGE ( 'NONE', *, *, #6986, .T. ) ;
#15974 = CARTESIAN_POINT ( 'NONE',  ( 26.45077056032005913, -6.103994453487816330, -7.939653947423664704 ) ) ;
#15975 = B_SPLINE_CURVE_WITH_KNOTS ( 'NONE', 3,
 ( #3890, #1170, #6690, #8146, #17203, #15296, #10086, #4746 ),
 .UNSPECIFIED., .F., .F.,
 ( 4, 2, 2, 4 ),
 ( 0.8481424625553403152, 0.8776269672338687933, 0.9071114719123971604, 0.9660804812694540056 ),
 .UNSPECIFIED. ) ;
#15976 = CARTESIAN_POINT ( 'NONE',  ( 31.67382807612511542, -6.101689702897060030, -6.861505862736167138 ) ) ;
#15977 = ORIENTED_EDGE ( 'NONE', *, *, #698, .T. ) ;
#15978 = PLANE ( 'NONE',  #6607 ) ;
#15979 = VECTOR ( 'NONE', #2898, 999.9999999999998863 ) ;
#15980 = CARTESIAN_POINT ( 'NONE',  ( 26.55511561737958814, -2.656761491791831187, 4.533357778048667797 ) ) ;
#15981 = EDGE_LOOP ( 'NONE', ( #5714, #1517, #11946, #322 ) ) ;
#15982 = CARTESIAN_POINT ( 'NONE',  ( 29.23078034989804763, -4.515117109069654688, -8.283357778048662468 ) ) ;
#15983 = VECTOR ( 'NONE', #12311, 1000.000000000000000 ) ;
#15984 = VECTOR ( 'NONE', #10526, 1000.000000000000227 ) ;
#15985 = CARTESIAN_POINT ( 'NONE',  ( 32.65880277236253448, -4.102108105263264193, -7.939653947423662039 ) ) ;
#15986 = ORIENTED_EDGE ( 'NONE', *, *, #15055, .F. ) ;
#15987 = CARTESIAN_POINT ( 'NONE',  ( 5.499998817156067865, -20.49639288455253450, 6.000000000000000000 ) ) ;
#15988 = CARTESIAN_POINT ( 'NONE',  ( 26.01345249736710841, -4.876873030332669501, -8.181274557237335543 ) ) ;
#15989 = FACE_OUTER_BOUND ( 'NONE', #1908, .T. ) ;
#15990 = AXIS2_PLACEMENT_3D ( 'NONE', #8447, #15164, #197 ) ;
#15991 = CARTESIAN_POINT ( 'NONE',  ( -2.016448651773435938E-27, -20.49999999999999645, -6.000000000000000000 ) ) ;
#15992 = EDGE_CURVE ( 'NONE', #5342, #15678, #11350, .T. ) ;
#15993 = CARTESIAN_POINT ( 'NONE',  ( 29.81239362717914787, -2.264323817775507397, -4.533357778048659803 ) ) ;
#15994 = CARTESIAN_POINT ( 'NONE',  ( 26.84461768998868436, -2.294720455324902542, -5.783357778048658027 ) ) ;
#15995 = VECTOR ( 'NONE', #11544, 1000.000000000000227 ) ;
#15996 = CARTESIAN_POINT ( 'NONE',  ( -32.93004296264518160, -25.68697430340739629, -12.29384923381406658 ) ) ;
#15997 = PLANE ( 'NONE',  #14176 ) ;
#15998 = CARTESIAN_POINT ( 'NONE',  ( 4.081988505578530102, 17.67880197223097127, -16.99999999999999645 ) ) ;
#15999 = CARTESIAN_POINT ( 'NONE',  ( 27.29063000668916672, -2.568146533142987575, -4.533357778048659803 ) ) ;
#16000 = CARTESIAN_POINT ( 'NONE',  ( 30.75425665345519732, -2.450656702321377001, -4.705209693361161349 ) ) ;
#16001 = CONICAL_SURFACE ( 'NONE', #2669, 9.500000000000001776, 0.7853981633974465026 ) ;
#16002 = ORIENTED_EDGE ( 'NONE', *, *, #3556, .T. ) ;
#16003 = CARTESIAN_POINT ( 'NONE',  ( -20.00000000000000000, 7.999999999999996447, 0.000000000000000000 ) ) ;
#16004 = CARTESIAN_POINT ( 'NONE',  ( -20.00000000000000355, 7.999999999999996447, 6.000000000000000000 ) ) ;
#16005 = CARTESIAN_POINT ( 'NONE',  ( -35.74085044863416272, -23.57886868891566223, 11.27079897466147607 ) ) ;
#16006 = ORIENTED_EDGE ( 'NONE', *, *, #10483, .T. ) ;
#16007 = CARTESIAN_POINT ( 'NONE',  ( 25.77386970449396486, -2.888308184441639170, 4.943601421580931188 ) ) ;
#16008 = DIRECTION ( 'NONE',  ( -0.8660254037844432595, -0.4999999999999921174, 0.000000000000000000 ) ) ;
#16009 = CARTESIAN_POINT ( 'NONE',  ( 25.76524775868381667, -2.816745038626284892, -5.277258820486252944 ) ) ;
#16010 = CARTESIAN_POINT ( 'NONE',  ( 32.30426898124760982, -6.025734024055190652, -6.861505862736167138 ) ) ;
#16011 = EDGE_CURVE ( 'NONE', #6049, #10596, #8116, .T. ) ;
#16012 = CARTESIAN_POINT ( 'NONE',  ( 33.15485366002904755, -6.560422763297783177, 5.783357778048664244 ) ) ;
#16013 = AXIS2_PLACEMENT_3D ( 'NONE', #8569, #16933, #12838 ) ;
#16014 = VECTOR ( 'NONE', #10232, 1000.000000000000000 ) ;
#16015 = CARTESIAN_POINT ( 'NONE',  ( 27.73348320195396965, -4.695511846111656062, -3.283357778048664688 ) ) ;
#16016 = DIRECTION ( 'NONE',  ( 0.000000000000000000, -1.000000000000000000, -3.469446951953614189E-16 ) ) ;
#16017 = ITEM_DEFINED_TRANSFORMATION ( 'NONE', 'NONE', #17274,  #3575 ) ;
#16018 = DIRECTION ( 'NONE',  ( 0.000000000000000000, 0.000000000000000000, 1.000000000000000000 ) ) ;
#16019 = CYLINDRICAL_SURFACE ( 'NONE', #6570, 2.500000000000001776 ) ;
#16020 = ORIENTED_EDGE ( 'NONE', *, *, #15089, .F. ) ;
#16021 = B_SPLINE_CURVE_WITH_KNOTS ( 'NONE', 3,
 ( #8258, #17903, #1103, #5083, #17648 ),
 .UNSPECIFIED., .F., .F.,
 ( 4, 1, 4 ),
 ( 0.000000000000000000, 0.002309401076758504923, 0.004618802153517009845 ),
 .UNSPECIFIED. ) ;
#16022 = CARTESIAN_POINT ( 'NONE',  ( 28.91999743871649997, -5.806501378023834370, -3.627061608673668225 ) ) ;
#16023 = FACE_OUTER_BOUND ( 'NONE', #17927, .T. ) ;
#16024 = CARTESIAN_POINT ( 'NONE',  ( 28.29630561643014275, -19.54286113573893502, -13.63865706309495884 ) ) ;
#16025 = AXIS2_PLACEMENT_3D ( 'NONE', #11381, #11184, #15483 ) ;
#16026 = CARTESIAN_POINT ( 'NONE',  ( 26.49878054387835746, -2.963357534503999968, 6.861505862736166250 ) ) ;
#16027 = VECTOR ( 'NONE', #7858, 1000.000000000000000 ) ;
#16028 = ORIENTED_EDGE ( 'NONE', *, *, #7913, .T. ) ;
#16029 = DIRECTION ( 'NONE',  ( 0.06446199418653537905, 0.9979201627913403261, 4.248110196704583871E-22 ) ) ;
#16030 = EDGE_LOOP ( 'NONE', ( #4217, #6684, #6680, #564 ) ) ;
#16031 = CARTESIAN_POINT ( 'NONE',  ( 31.54230778485832332, -2.355712103769039611, 6.861505862736166250 ) ) ;
#16032 = CARTESIAN_POINT ( 'NONE',  ( 28.09753128235661279, -6.832371619143005503, 7.033357778048657138 ) ) ;
#16033 = CARTESIAN_POINT ( 'NONE',  ( -2.344047193898589398, -3.265465875126477346, -8.103564206381888188E-15 ) ) ;
#16034 = ORIENTED_EDGE ( 'NONE', *, *, #1700, .T. ) ;
#16035 = CARTESIAN_POINT ( 'NONE',  ( -11.54660026683835383, -4.788112600790469742, -8.722503561260788629 ) ) ;
#16036 = DIRECTION ( 'NONE',  ( 0.000000000000000000, 0.000000000000000000, -1.000000000000000000 ) ) ;
#16037 = VERTEX_POINT ( 'NONE', #13650 ) ;
#16039 = AXIS2_PLACEMENT_3D ( 'NONE', #8710, #5970, #1922 ) ;
#16038 = FACE_OUTER_BOUND ( 'NONE', #15470, .T. ) ;
#16040 = CARTESIAN_POINT ( 'NONE',  ( 33.44685390376565692, -4.007163506710925027, -7.939653947423662039 ) ) ;
#16041 = VERTEX_POINT ( 'NONE', #1238 ) ;
#16042 = CARTESIAN_POINT ( 'NONE',  ( 31.51621784984448738, -6.120678622607529817, -6.861505862736166250 ) ) ;
#16043 = CARTESIAN_POINT ( 'NONE',  ( 28.74176732417158320, -7.092112515190875044, -5.783357778048657138 ) ) ;
#16044 = CARTESIAN_POINT ( 'NONE',  ( 39.99999999999999289, 2.789133085058097101E-16, -2.055000000000000160 ) ) ;
#16045 =( NAMED_UNIT ( * ) PLANE_ANGLE_UNIT ( ) SI_UNIT ( $, .RADIAN. ) );
#16046 = CARTESIAN_POINT ( 'NONE',  ( 29.01637427789896151, -7.048830937829683840, -5.783357778048668685 ) ) ;
#16047 = CARTESIAN_POINT ( 'NONE',  ( 32.92339180097568629, -5.524043937428110063, -3.283357778048667797 ) ) ;
#16048 = DIRECTION ( 'NONE',  ( -0.000000000000000000, -0.000000000000000000, -1.000000000000000000 ) ) ;
#16049 = DIRECTION ( 'NONE',  ( 0.000000000000000000, 0.000000000000000000, 1.000000000000000000 ) ) ;
#16050 = CARTESIAN_POINT ( 'NONE',  ( 32.27410075503257758, -1.240829931302721345, 5.783357778048668685 ) ) ;
#16051 = ORIENTED_EDGE ( 'NONE', *, *, #7413, .F. ) ;
#16052 = ORIENTED_EDGE ( 'NONE', *, *, #5310, .F. ) ;
#16053 = EDGE_LOOP ( 'NONE', ( #12457, #16951, #2206, #7453 ) ) ;
#16054 = LINE ( 'NONE', #3623, #12664 ) ;
#16055 = CARTESIAN_POINT ( 'NONE',  ( 32.08959525433819238, -2.916745304588811205, 3.627061608673666449 ) ) ;
#16056 = EDGE_LOOP ( 'NONE', ( #12360, #4937, #9053, #9976 ) ) ;
#16057 =( LENGTH_UNIT ( ) NAMED_UNIT ( * ) SI_UNIT ( .MILLI., .METRE. ) );
#16058 = CARTESIAN_POINT ( 'NONE',  ( 29.15568435273173264, -2.343444316361667834, -7.033357778048658027 ) ) ;
#16059 = DIRECTION ( 'NONE',  ( -1.000000000000000000, -0.000000000000000000, -0.000000000000000000 ) ) ;
#16060 = CARTESIAN_POINT ( 'NONE',  ( 28.30694982360322953, -3.372479377640031473, -7.939653947423660263 ) ) ;
#16061 = CARTESIAN_POINT ( 'NONE',  ( 30.66124439477291475, -6.860853434864224276, -6.453230759126470595 ) ) ;
#16062 = CARTESIAN_POINT ( 'NONE',  ( 35.46635924378174565, -16.45598204045931823, -11.37070560279563480 ) ) ;
#16064 = ADVANCED_FACE ( 'NONE', ( #10896 ), #8182, .T. ) ;
#16063 = CARTESIAN_POINT ( 'NONE',  ( 32.90454166015506132, -1.164874252460851300, -5.783357778048658027 ) ) ;
#16065 = CARTESIAN_POINT ( 'NONE',  ( 34.91600907648203389, -11.88801210197604341, 12.00000000000000000 ) ) ;
#16066 = UNCERTAINTY_MEASURE_WITH_UNIT (LENGTH_MEASURE( 1.000000000000000082E-05 ), #3046, 'distance_accuracy_value', 'NONE');
#16067 = CARTESIAN_POINT ( 'NONE',  ( 22.22415228291801981, -10.00312865908476567, 15.08655899088414820 ) ) ;
#16068 = FILL_AREA_STYLE_COLOUR ( '', #7273 ) ;
#16069 = CARTESIAN_POINT ( 'NONE',  ( 26.97161122272022382, -2.906390775372597712, -4.705209693361161349 ) ) ;
#16070 = CARTESIAN_POINT ( 'NONE',  ( 32.32618902979206865, -6.650063623909865385, -5.783357778048669573 ) ) ;
#16071 = ORIENTED_EDGE ( 'NONE', *, *, #3114, .T. ) ;
#16072 = EDGE_CURVE ( 'NONE', #16640, #9754, #9003, .T. ) ;
#16073 = LINE ( 'NONE', #913, #16463 ) ;
#16074 = CARTESIAN_POINT ( 'NONE',  ( 0.000000000000000000, -1.178949249685213863, 2.042000000000001148 ) ) ;
#16075 = ORIENTED_EDGE ( 'NONE', *, *, #3369, .T. ) ;
#16076 = CARTESIAN_POINT ( 'NONE',  ( 26.32044349065828115, -7.243571858916999950, 4.872287503353643245 ) ) ;
#16077 = CARTESIAN_POINT ( 'NONE',  ( 31.28415083292585663, -5.521667582366822202, -3.627061608673667781 ) ) ;
#16078 = ORIENTED_EDGE ( 'NONE', *, *, #182, .F. ) ;
#16079 = CYLINDRICAL_SURFACE ( 'NONE', #15081, 4.250000000000000000 ) ;
#16080 = CARTESIAN_POINT ( 'NONE',  ( 25.90419076669538256, -3.969988049114259177, -7.913474645583921330 ) ) ;
#16081 = LINE ( 'NONE', #7455, #17117 ) ;
#16082 = ADVANCED_FACE ( 'NONE', ( #15639 ), #11538, .T. ) ;
#16083 = CARTESIAN_POINT ( 'NONE',  ( 1.296864337298335788E-21, -1.182044466681725685E-21, -6.899999999999998579 ) ) ;
#16084 = CARTESIAN_POINT ( 'NONE',  ( 31.84257795004535652, -2.746633492292519296, -3.283357778048662023 ) ) ;
#16085 = ORIENTED_EDGE ( 'NONE', *, *, #659, .F. ) ;
#16086 = CARTESIAN_POINT ( 'NONE',  ( 25.71072941247523502, -3.058302133056337357, -4.705209693361161349 ) ) ;
#16087 = DIRECTION ( 'NONE',  ( 0.000000000000000000, 0.000000000000000000, 1.000000000000000000 ) ) ;
#16088 = DIRECTION ( 'NONE',  ( 0.000000000000000000, 0.000000000000000000, -1.000000000000000000 ) ) ;
#16089 = DIRECTION ( 'NONE',  ( 0.000000000000000000, 0.000000000000000000, 1.000000000000000000 ) ) ;
#16090 = CARTESIAN_POINT ( 'NONE',  ( 28.28511899221430070, -4.629050627332469858, -3.283357778048664688 ) ) ;
#16091 = CARTESIAN_POINT ( 'NONE',  ( 32.56242593318006584, -2.859778545457409837, -7.939653947423660263 ) ) ;
#16092 = EDGE_CURVE ( 'NONE', #15670, #16642, #17831, .T. ) ;
#16093 = EDGE_LOOP ( 'NONE', ( #5896, #5082, #8960, #4409 ) ) ;
#16094 = ORIENTED_EDGE ( 'NONE', *, *, #1356, .F. ) ;
#16095 = CARTESIAN_POINT ( 'NONE',  ( -36.27615609941022257, -23.17738945083361557, 12.00000000000000000 ) ) ;
#16096 = MECHANICAL_DESIGN_GEOMETRIC_PRESENTATION_REPRESENTATION (  '', ( #3928 ), #15206 ) ;
#16097 = DIRECTION ( 'NONE',  ( -0.1196152422706597551, 0.9928203230275514102, 0.000000000000000000 ) ) ;
#16098 = CARTESIAN_POINT ( 'NONE',  ( 27.22618411036838637, -2.238552374514887866, 6.453230759126474148 ) ) ;
#16099 = EDGE_LOOP ( 'NONE', ( #11328, #5167, #15214, #13050 ) ) ;
#16100 = CARTESIAN_POINT ( 'NONE',  ( 25.94629020164263267, -4.319418220471660241, 3.500307223198195317 ) ) ;
#16101 = PLANE ( 'NONE',  #9874 ) ;
#16102 = CARTESIAN_POINT ( 'NONE',  ( 15.92260893619738837, -28.39189527176317540, -12.00000000000000000 ) ) ;
#16103 = CARTESIAN_POINT ( 'NONE',  ( 27.17934203385504333, -30.00000000000000355, -12.00000000000000000 ) ) ;
#16104 = VERTEX_POINT ( 'NONE', #5923 ) ;
#16105 = CARTESIAN_POINT ( 'NONE',  ( 28.79925754835455010, -6.020920669644549861, -8.283357778048662468 ) ) ;
#16106 = DIRECTION ( 'NONE',  ( -0.9928203230275511881, -0.1196152422706614482, -0.000000000000000000 ) ) ;
#16107 = CARTESIAN_POINT ( 'NONE',  ( -34.91600907648203389, -11.88801210197604341, 11.56671555609732671 ) ) ;
#16108 = LINE ( 'NONE', #6488, #9746 ) ;
#16109 = EDGE_LOOP ( 'NONE', ( #7874, #14047, #4709, #10171 ) ) ;
#16110 = CARTESIAN_POINT ( 'NONE',  ( 29.02054416436834217, -2.659534819136519790, -4.705209693361160461 ) ) ;
#16111 = CARTESIAN_POINT ( 'NONE',  ( 33.40660799972355477, 0.6401911282994665608, -5.783357778048661579 ) ) ;
#16112 = CARTESIAN_POINT ( 'NONE',  ( 33.59503905791412137, -1.808589744724287129, 7.033357778048666020 ) ) ;
#16113 = CARTESIAN_POINT ( 'NONE',  ( 25.86833963875586306, -3.039313213345869791, 6.861505862736166250 ) ) ;
#16114 = VERTEX_POINT ( 'NONE', #15541 ) ;
#16115 = EDGE_CURVE ( 'NONE', #8269, #3859, #1874, .T. ) ;
#16116 = ORIENTED_EDGE ( 'NONE', *, *, #961, .T. ) ;
#16117 = VERTEX_POINT ( 'NONE', #6010 ) ;
#16118 = CARTESIAN_POINT ( 'NONE',  ( 28.54354359905709870, -7.105797696961086096, 5.783357778048657138 ) ) ;
#16119 = CARTESIAN_POINT ( 'NONE',  ( 27.73348320195396965, -4.695511846111656062, 8.283357778048662468 ) ) ;
#16120 = CARTESIAN_POINT ( 'NONE',  ( -4.000000000000000888, -2.309401076758508253, -3.204269196027527133 ) ) ;
#16121 = ORIENTED_EDGE ( 'NONE', *, *, #9154, .F. ) ;
#16122 = CARTESIAN_POINT ( 'NONE',  ( 2.500000000000000888, 0.000000000000000000, -25.03750572909317285 ) ) ;
#16123 = DIRECTION ( 'NONE',  ( 0.000000000000000000, 0.5027044994213119011, 0.8644583195629320649 ) ) ;
#16124 = EDGE_CURVE ( 'NONE', #16117, #4517, #11251, .T. ) ;
#16125 = CARTESIAN_POINT ( 'NONE',  ( 26.31556265977298992, -7.384422263489805793, -5.783357778048663356 ) ) ;
#16126 = CARTESIAN_POINT ( 'NONE',  ( 32.32618902979206865, -6.650063623909865385, -5.783357778048669573 ) ) ;
#16127 = CARTESIAN_POINT ( 'NONE',  ( 32.79901970863393501, -6.593096864778464017, -5.783357778048668685 ) ) ;
#16128 = CARTESIAN_POINT ( 'NONE',  ( 28.43075721014566781, -2.093425104433228157, -6.453230759126469707 ) ) ;
#16129 = FACE_OUTER_BOUND ( 'NONE', #13883, .T. ) ;
#16130 = CARTESIAN_POINT ( 'NONE',  ( 28.97253418081003673, -5.800171738120336151, -7.939653947423664704 ) ) ;
#16131 = LINE ( 'NONE', #9961, #2678 ) ;
#16132 = CARTESIAN_POINT ( 'NONE',  ( -10.50000000000000000, 0.000000000000000000, -4.000000000000000000 ) ) ;
#16133 = CARTESIAN_POINT ( 'NONE',  ( 25.71748644841968456, -2.420320648352051851, -5.783357778048663356 ) ) ;
#16134 = CARTESIAN_POINT ( 'NONE',  ( 29.98885399772409954, -6.604504582617394703, 7.033357778048657138 ) ) ;
#16135 = EDGE_CURVE ( 'NONE', #9754, #1502, #12698, .T. ) ;
#16136 = EDGE_LOOP ( 'NONE', ( #16959, #417, #1867, #13753 ) ) ;
#16137 = B_SPLINE_CURVE_WITH_KNOTS ( 'NONE', 3,
 ( #13481, #6226, #8948, #17414, #17685 ),
 .UNSPECIFIED., .F., .F.,
 ( 4, 1, 4 ),
 ( 0.9660804812694540056, 0.9703207337145166589, 0.9745609861595793122 ),
 .UNSPECIFIED. ) ;
#16138 = ORIENTED_EDGE ( 'NONE', *, *, #1767, .F. ) ;
#16139 = ORIENTED_EDGE ( 'NONE', *, *, #2895, .F. ) ;
#16140 = CARTESIAN_POINT ( 'NONE',  ( 26.31556265977298992, -7.384422263489805793, 5.783357778048663356 ) ) ;
#16141 = CARTESIAN_POINT ( 'NONE',  ( 31.43723430067123914, -2.368371383576012956, 4.705209693361168455 ) ) ;
#16142 = ORIENTED_EDGE ( 'NONE', *, *, #11253, .T. ) ;
#16143 = CARTESIAN_POINT ( 'NONE',  ( -2.016448651773435938E-27, -20.49999999999999645, -13.00000000000000355 ) ) ;
#16144 = CARTESIAN_POINT ( 'NONE',  ( 36.27615609941022257, -23.17738945083361557, 0.000000000000000000 ) ) ;
#16145 = CARTESIAN_POINT ( 'NONE',  ( 27.29814976067589072, -3.294147343736874234, -8.283357778048660691 ) ) ;
#16146 = CARTESIAN_POINT ( 'NONE',  ( 30.60986983071443390, -4.348964061499348333, -3.627061608673664672 ) ) ;
#16147 = CARTESIAN_POINT ( 'NONE',  ( -5.500000000000000888, -20.49999999999999645, 12.00000000000000000 ) ) ;
#16148 = CARTESIAN_POINT ( 'NONE',  ( 31.88017671309158274, -6.376637546091784792, -4.533357778048668685 ) ) ;
#16149 = DIRECTION ( 'NONE',  ( 0.9928203230275510771, 0.1196152422706614621, -0.000000000000000000 ) ) ;
#16150 = CARTESIAN_POINT ( 'NONE',  ( 26.60838078660069428, -6.085005533777348319, -7.939653947423664704 ) ) ;
#16151 = CARTESIAN_POINT ( 'NONE',  ( 16.75000000000000000, -16.21813761408365195, 16.03574476417184513 ) ) ;
#16152 = CARTESIAN_POINT ( 'NONE',  ( 0.000000000000000000, 0.000000000000000000, 0.000000000000000000 ) ) ;
#16153 = CARTESIAN_POINT ( 'NONE',  ( 32.72003615946069743, -2.840789625746940938, -7.939653947423660263 ) ) ;
#16154 = CARTESIAN_POINT ( 'NONE',  ( 32.06767520579373354, -2.292415704734142690, -6.861505862736158257 ) ) ;
#16155 = ORIENTED_EDGE ( 'NONE', *, *, #15775, .T. ) ;
#16156 = AXIS2_PLACEMENT_3D ( 'NONE', #8530, #12520, #10 ) ;
#16157 = CARTESIAN_POINT ( 'NONE',  ( 26.02974819644417792, -2.720057890826728109, 7.033357778048666020 ) ) ;
#16158 = EDGE_CURVE ( 'NONE', #1034, #9766, #16312, .T. ) ;
#16159 = AXIS2_PLACEMENT_3D ( 'NONE', #13723, #2756, #2926 ) ;
#16160 = VERTEX_POINT ( 'NONE', #14375 ) ;
#16161 = CARTESIAN_POINT ( 'NONE',  ( 26.27749392786456895, -6.324743385012030927, 3.283357778048663356 ) ) ;
#16162 = CARTESIAN_POINT ( 'NONE',  ( 31.88814493096864311, -1.687075024589942407, -5.783357778048658915 ) ) ;
#16163 = ORIENTED_EDGE ( 'NONE', *, *, #16260, .T. ) ;
#16164 = DIRECTION ( 'NONE',  ( -0.9979201627913403261, 0.06446199418653535129, 0.000000000000000000 ) ) ;
#16165 = CARTESIAN_POINT ( 'NONE',  ( 26.10492286888475633, -5.636087676172646610, -8.120510362352304057 ) ) ;
#16166 = ADVANCED_FACE ( 'NONE', ( #4303 ), #14096, .F. ) ;
#16167 = DIRECTION ( 'NONE',  ( 0.9928203230275512992, 0.1196152422706610180, 4.006172263299093133E-17 ) ) ;
#16168 = CARTESIAN_POINT ( 'NONE',  ( 0.000000000000000000, 0.000000000000000000, -4.000000000000000000 ) ) ;
#16169 = CARTESIAN_POINT ( 'NONE',  ( 31.21213704492286212, -2.822589171134389563, -3.283357778048662023 ) ) ;
#16170 = AXIS2_PLACEMENT_3D ( 'NONE', #1858, #12807, #304 ) ;
#16171 = ORIENTED_EDGE ( 'NONE', *, *, #6062, .T. ) ;
#16172 = CARTESIAN_POINT ( 'NONE',  ( 32.79901970863393501, -6.593096864778464017, -5.783357778048668685 ) ) ;
#16173 = CARTESIAN_POINT ( 'NONE',  ( 25.97837335112617652, -4.585712065882579402, -3.626324104489874411 ) ) ;
#16174 = DIRECTION ( 'NONE',  ( 0.1196152422706596996, -0.9928203230275514102, 0.000000000000000000 ) ) ;
#16175 = DIRECTION ( 'NONE',  ( -0.000000000000000000, -0.000000000000000000, 1.000000000000000000 ) ) ;
#16176 = CARTESIAN_POINT ( 'NONE',  ( 29.14074637024071635, -5.979778010479330774, -3.283357778048667797 ) ) ;
#16177 = CARTESIAN_POINT ( 'NONE',  ( 32.16857880351144416, -6.669052543620333395, -5.783357778048668685 ) ) ;
#16178 = AXIS2_PLACEMENT_3D ( 'NONE', #8895, #1929, #6170 ) ;
#16179 = EDGE_CURVE ( 'NONE', #4780, #17008, #80, .T. ) ;
#16180 = AXIS2_PLACEMENT_3D ( 'NONE', #16774, #10131, #3261 ) ;
#16181 = ORIENTED_EDGE ( 'NONE', *, *, #11344, .T. ) ;
#16182 = DIRECTION ( 'NONE',  ( 0.000000000000000000, 1.000000000000000000, 0.000000000000000000 ) ) ;
#16183 = CARTESIAN_POINT ( 'NONE',  ( 34.43754810739937966, -7.916730809865823559, 5.783357778048663356 ) ) ;
#16184 = VECTOR ( 'NONE', #10568, 1000.000000000000000 ) ;
#16185 = EDGE_CURVE ( 'NONE', #5221, #11770, #13420, .T. ) ;
#16186 = VERTEX_POINT ( 'NONE', #1596 ) ;
#16187 = CARTESIAN_POINT ( 'NONE',  ( 25.88432464927661059, -3.805096980563281939, 3.751875008055423955 ) ) ;
#16188 = ADVANCED_FACE ( 'NONE', ( #7128 ), #12639, .F. ) ;
#16189 = LINE ( 'NONE', #3752, #5247 ) ;
#16190 = CARTESIAN_POINT ( 'NONE',  ( 33.30663696749426350, -1.516174747195734085, -5.783357778048658915 ) ) ;
#16191 = ORIENTED_EDGE ( 'NONE', *, *, #883, .T. ) ;
#16192 = CYLINDRICAL_SURFACE ( 'NONE', #15141, 2.000000000000001776 ) ;
#16193 = CARTESIAN_POINT ( 'NONE',  ( 28.83304567166618781, -6.743756660494150346, -7.033357778048666908 ) ) ;
#16194 = CARTESIAN_POINT ( 'NONE',  ( 26.01652455409633902, -4.902371455920926380, -5.783357778048663356 ) ) ;
#16195 = FACE_OUTER_BOUND ( 'NONE', #2008, .T. ) ;
#16196 = DIRECTION ( 'NONE',  ( -0.000000000000000000, -0.000000000000000000, -1.000000000000000000 ) ) ;
#16197 = CARTESIAN_POINT ( 'NONE',  ( 30.92509028327567933, -4.310986222078405206, -7.939653947423662039 ) ) ;
#16198 = AXIS2_PLACEMENT_3D ( 'NONE', #12032, #17794, #15118 ) ;
#16199 = CARTESIAN_POINT ( 'NONE',  ( 33.38562051666750818, -5.268481986227246061, -7.939653947423664704 ) ) ;
#16200 = CARTESIAN_POINT ( 'NONE',  ( 26.12396475346091052, -21.64644127732803014, -14.20549555447399470 ) ) ;
#16201 = CARTESIAN_POINT ( 'NONE',  ( 31.21213704492286212, -2.822589171134389563, 8.283357778048664244 ) ) ;
#16202 =( REPRESENTATION_RELATIONSHIP ('NONE','NONE', #3227, #691 ) REPRESENTATION_RELATIONSHIP_WITH_TRANSFORMATION ( #4836 )SHAPE_REPRESENTATION_RELATIONSHIP( ) );
#16203 = VERTEX_POINT ( 'NONE', #10358 ) ;
#16204 = AXIS2_PLACEMENT_3D ( 'NONE', #6115, #11643, #17210 ) ;
#16205 = CARTESIAN_POINT ( 'NONE',  ( 30.29464937815318493, -4.386941900920275472, 3.627061608673664228 ) ) ;
#16206 = CARTESIAN_POINT ( 'NONE',  ( -27.11337801594864061, -11.49512195020015604, 13.95421129451976050 ) ) ;
#16207 = CARTESIAN_POINT ( 'NONE',  ( 26.31556265977298992, -7.384422263489805793, -5.783357778048663356 ) ) ;
#16208 = EDGE_LOOP ( 'NONE', ( #152, #17216, #12651, #10414 ) ) ;
#16209 = VECTOR ( 'NONE', #8283, 1000.000000000000000 ) ;
#16210 = LINE ( 'NONE', #3413, #16810 ) ;
#16211 = DIRECTION ( 'NONE',  ( -1.000000000000000000, 0.000000000000000000, 0.000000000000000000 ) ) ;
#16212 = CARTESIAN_POINT ( 'NONE',  ( 29.17398450417959310, -7.029842018119214941, -5.783357778048669573 ) ) ;
#16213 = EDGE_CURVE ( 'NONE', #16114, #1819, #16595, .T. ) ;
#16214 = CARTESIAN_POINT ( 'NONE',  ( 31.05948030073166066, -1.776715885202022394, 5.783357778048665132 ) ) ;
#16215 = DIRECTION ( 'NONE',  ( -0.1196152422706614343, 0.9928203230275510771, 0.000000000000000000 ) ) ;
#16216 =( NAMED_UNIT ( * ) PLANE_ANGLE_UNIT ( ) SI_UNIT ( $, .RADIAN. ) );
#16217 = CARTESIAN_POINT ( 'NONE',  ( 27.75549246765397271, -7.200742295513423485, 5.783357778048658027 ) ) ;
#16218 = PRODUCT_DEFINITION_SHAPE ( 'NONE', 'NONE',  #16665 ) ;
#16219 = CARTESIAN_POINT ( 'NONE',  ( 33.18226487515251932, -2.585227674546096477, 8.283357778048666020 ) ) ;
#16220 = CARTESIAN_POINT ( 'NONE',  ( 8.472608240843633681E-22, -7.722472891792491889E-22, -7.794427190999915211 ) ) ;
#16221 = CARTESIAN_POINT ( 'NONE',  ( 28.76917853929504432, -3.116917426439186123, 8.283357778048664244 ) ) ;
#16222 = AXIS2_PLACEMENT_3D ( 'NONE', #4057, #15119, #2706 ) ;
#16223 = ORIENTED_EDGE ( 'NONE', *, *, #9120, .T. ) ;
#16224 = VERTEX_POINT ( 'NONE', #11723 ) ;
#16225 = CARTESIAN_POINT ( 'NONE',  ( 32.54050588463559990, -2.235448945602741766, 4.705209693361167567 ) ) ;
#16226 = VECTOR ( 'NONE', #17017, 1000.000000000000000 ) ;
#16227 = CARTESIAN_POINT ( 'NONE',  ( 31.67382807612511542, -6.101689702897060030, 4.705209693361159573 ) ) ;
#16228 = ORIENTED_EDGE ( 'NONE', *, *, #16719, .T. ) ;
#16229 = CARTESIAN_POINT ( 'NONE',  ( 50.00000000000000000, -16.03270077640482683, -5.537981825772250843 ) ) ;
#16230 = DIRECTION ( 'NONE',  ( 1.000000000000000000, 0.000000000000000000, 0.000000000000000000 ) ) ;
#16231 = DIRECTION ( 'NONE',  ( -0.9928203230275511881, -0.1196152422706610041, -4.006172263299093133E-17 ) ) ;
#16232 = CARTESIAN_POINT ( 'NONE',  ( 29.34898802046944155, -4.500875419183088866, -3.627061608673664672 ) ) ;
#16233 = DIRECTION ( 'NONE',  ( 1.000000000000000000, 0.000000000000000000, 0.000000000000000000 ) ) ;
#16234 = CIRCLE ( 'NONE', #12725, 5.560781378645573980 ) ;
#16235 = CARTESIAN_POINT ( 'NONE',  ( 33.40745134805642635, -4.011910736534825439, -3.283357778048664688 ) ) ;
#16236 = DIRECTION ( 'NONE',  ( 0.000000000000000000, 0.000000000000000000, 1.000000000000000000 ) ) ;
#16237 = EDGE_CURVE ( 'NONE', #2633, #2890, #10452, .T. ) ;
#16238 = CARTESIAN_POINT ( 'NONE',  ( 27.77288575766320378, -4.690764616287755651, -7.939653947423662039 ) ) ;
#16239 = CARTESIAN_POINT ( 'NONE',  ( 29.71979337562451207, -1.938121702948446323, 5.783357778048662468 ) ) ;
#16240 = EDGE_CURVE ( 'NONE', #6677, #3366, #14840, .T. ) ;
#16241 = VERTEX_POINT ( 'NONE', #15912 ) ;
#16242 = CARTESIAN_POINT ( 'NONE',  ( 30.28142597461332741, -2.507623461452779701, -4.705209693361160461 ) ) ;
#16243 = AXIS2_PLACEMENT_3D ( 'NONE', #4917, #943, #11804 ) ;
#16244 = CARTESIAN_POINT ( 'NONE',  ( 30.40841950734487753, -3.119293781500474427, -3.627061608673662008 ) ) ;
#16245 = ORIENTED_EDGE ( 'NONE', *, *, #3357, .F. ) ;
#16246 = CARTESIAN_POINT ( 'NONE',  ( 31.29094215978502902, -2.813094711071706389, 8.283357778048666020 ) ) ;
#16247 = CARTESIAN_POINT ( 'NONE',  ( -45.00000000000000711, -16.03270077640482683, -5.537981825772250843 ) ) ;
#16248 = EDGE_LOOP ( 'NONE', ( #13312, #2140, #13663, #13056 ) ) ;
#16249 = CARTESIAN_POINT ( 'NONE',  ( 30.64918316926811315, -2.463315982128351678, 4.705209693361167567 ) ) ;
#16250 = CARTESIAN_POINT ( 'NONE',  ( 28.23249303296521617, -2.754479417688857179, -4.705209693361161349 ) ) ;
#16251 = CARTESIAN_POINT ( 'NONE',  ( -14.00000000000000178, 0.000000000000000000, 8.700000000000001066 ) ) ;
#16252 = VECTOR ( 'NONE', #6708, 1000.000000000000114 ) ;
#16253 = LINE ( 'NONE', #5428, #4962 ) ;
#16254 = CARTESIAN_POINT ( 'NONE',  ( 25.95642634701329499, -4.403549397486667516, 7.880302681851837576 ) ) ;
#16255 = AXIS2_PLACEMENT_3D ( 'NONE', #1926, #14340, #7446 ) ;
#16256 = CARTESIAN_POINT ( 'NONE',  ( 4.175647895129167786, -2.207990717223094812, -3.169390900447852655 ) ) ;
#16257 = ADVANCED_FACE ( 'NONE', ( #14466 ), #16192, .F. ) ;
#16258 = CARTESIAN_POINT ( 'NONE',  ( 32.82573654529290508, -1.174368712523534475, -5.783357778048658027 ) ) ;
#16259 = CIRCLE ( 'NONE', #898, 9.500000000000000000 ) ;
#16260 = EDGE_CURVE ( 'NONE', #13000, #10514, #14582, .T. ) ;
#16261 = ORIENTED_EDGE ( 'NONE', *, *, #17763, .F. ) ;
#16262 = CARTESIAN_POINT ( 'NONE',  ( 32.67202617590239555, -5.981426544730773287, -4.705209693361168455 ) ) ;
#16263 = CARTESIAN_POINT ( 'NONE',  ( 0.000000000000000000, 0.000000000000000000, -3.000000000000002665 ) ) ;
#16264 = CARTESIAN_POINT ( 'NONE',  ( 1.312671235360370892, 3.860931062424219462, -0.05923475698270563861 ) ) ;
#16265 = CARTESIAN_POINT ( 'NONE',  ( 3.453019673806209333, 2.625200315326833067, -3.235259548910759619 ) ) ;
#16266 = CARTESIAN_POINT ( 'NONE',  ( -1.287221018261747618, -3.875624752117063920, -3.130620751971695093 ) ) ;
#16267 = CARTESIAN_POINT ( 'NONE',  ( 33.42946061375642586, -6.517141185936593750, -5.783357778048668685 ) ) ;
#16268 = VECTOR ( 'NONE', #16777, 1000.000000000000000 ) ;
#16269 = EDGE_CURVE ( 'NONE', #15926, #14747, #11064, .T. ) ;
#16270 = CIRCLE ( 'NONE', #6695, 2.000000000000001776 ) ;
#16271 = AXIS2_PLACEMENT_3D ( 'NONE', #9423, #9680, #12249 ) ;
#16272 = FACE_OUTER_BOUND ( 'NONE', #2821, .T. ) ;
#16273 = CARTESIAN_POINT ( 'NONE',  ( 33.60446413004628141, -3.988174587000466342, -3.627061608673664672 ) ) ;
#16274 = ORIENTED_EDGE ( 'NONE', *, *, #5934, .T. ) ;
#16275 =( LENGTH_UNIT ( ) NAMED_UNIT ( * ) SI_UNIT ( .MILLI., .METRE. ) );
#16276 = LINE ( 'NONE', #13010, #5823 ) ;
#16277 = DIRECTION ( 'NONE',  ( 0.000000000000000000, 0.000000000000000000, 1.000000000000000000 ) ) ;
#16278 = FACE_OUTER_BOUND ( 'NONE', #10688, .T. ) ;
#16279 = PRESENTATION_LAYER_ASSIGNMENT (  '', '', ( #6420 ) ) ;
#16280 = EDGE_CURVE ( 'NONE', #11429, #1653, #2145, .T. ) ;
#16281 = CARTESIAN_POINT ( 'NONE',  ( 26.69778786461289855, -6.274106265784127778, -3.283357778048667797 ) ) ;
#16282 = DIRECTION ( 'NONE',  ( 0.9928203230275510771, 0.1196152422706609902, 4.006172263299092517E-17 ) ) ;
#16283 = CYLINDRICAL_SURFACE ( 'NONE', #15628, 2.500000000000000000 ) ;
#16284 = FACE_OUTER_BOUND ( 'NONE', #7979, .T. ) ;
#16285 = CARTESIAN_POINT ( 'NONE',  ( 26.05393439953038381, -7.587479618990243146, -6.529799540429926274 ) ) ;
#16286 = VECTOR ( 'NONE', #7990, 1000.000000000000000 ) ;
#16287 = CARTESIAN_POINT ( 'NONE',  ( 33.40745134805642635, -4.011910736534825439, 8.283357778048662468 ) ) ;
#16288 = CARTESIAN_POINT ( 'NONE',  ( 32.50309786422735669, -5.574681056656012323, 3.283357778048663800 ) ) ;
#16289 = EDGE_CURVE ( 'NONE', #9288, #8961, #13512, .T. ) ;
#16290 = TOROIDAL_SURFACE ( 'NONE', #11031, 12.70000000000000284, 0.9000000000000003553 ) ;
#16291 = ORIENTED_EDGE ( 'NONE', *, *, #5483, .F. ) ;
#16292 = CARTESIAN_POINT ( 'NONE',  ( 29.67743187657054449, -6.342216019229654833, 6.861505862736157368 ) ) ;
#16293 = FILL_AREA_STYLE_COLOUR ( '', #1469 ) ;
#16294 = CARTESIAN_POINT ( 'NONE',  ( 21.03881409870396624, -22.15596512169676302, 15.31966522629967464 ) ) ;
#16295 = ORIENTED_EDGE ( 'NONE', *, *, #10315, .F. ) ;
#16296 = TOROIDAL_SURFACE ( 'NONE', #11941, 10.40000000000000036, 0.9000000000000003553 ) ;
#16297 = FACE_OUTER_BOUND ( 'NONE', #2801, .T. ) ;
#16298 = DIRECTION ( 'NONE',  ( 5.026720092345836698E-22, -4.581671729415424240E-22, 1.000000000000000000 ) ) ;
#16299 = CARTESIAN_POINT ( 'NONE',  ( 31.65190802758064592, -5.477360103042387074, -7.939653947423664704 ) ) ;
#16300 =( BOUNDED_SURFACE ( )  B_SPLINE_SURFACE ( 1, 2, ( 
 ( #2344, #11838, #17415, #14594, #11663, #10561, #16040, #974, #10476, #3334, #615, #4769, #10294, #15844, #3416, #6501, #3610, #877, #11747, #9131, #8949, #7862, #14490, #8864, #2169, #7769, #14671, #17316, #2251, #6410, #11929, #2074, #17517, #16126, #3686, #9210, #14759, #13393, #12017, #10897, #13482, #13820, #16466, #16299, #1407, #2426, #15187, #13739, #5207, #8290, #12102, #16388, #1320, #5470, #3869, #3950, #10991, #6930, #13563, #9301, #10727, #8211, #17937, #9638, #4035, #9552, #3778, #16549, #8119, #13651, #1058, #5294, #50, #14842, #6579, #9381, #5381, #12462, #2591, #5561, #14924, #17686, #12291, #2502, #1239, #1142, #8026, #6761, #6668, #6843, #12196, #17777, #2682, #16212, #10815, #2772, #7950, #9465, #15005, #17860, #15097, #12371, #4133, #3126, #4304, #8659, #15893, #7129, #3465, #17015, #14014, #13169, #4568, #5739, #9719, #9816, #7039, #2851, #14542, #745, #14187, #13911, #9910, #8478, #8997, #2124, #12554, #15367, #1504, #325, #7646, #138, #4483, #11080, #1597, #7308, #5650, #3043, #16644, #1780, #9998, #15542, #5831, #12829, #8379, #4219, #12640, #11252, #420, #11161, #4395, #229, #15270, #16732, #2948 ),
 ( #5924, #10337, #11356, #16926, #16831, #11448, #8564, #14097, #15458, #1683, #7217, #12729, #14631, #13250, #13440, #16258, #13613, #2470, #9345, #1020, #14966, #7907, #17562, #3832, #11979, #835, #3563, #14716, #2299, #9255, #3732, #10524, #3652, #14884, #5081, #6362, #9090, #16084, #11886, #10601, #2550, #5166, #17645, #10774, #7992, #17465, #7726, #17371, #8077, #16169, #9173, #12058, #6270, #2212, #4905, #16355, #7817, #13347, #4997, #14800, #927, #6461, #11792, #13526, #10431, #5254, #2391, #6543, #10682, #1100, #6624, #12152, #3915, #17734, #15993, #9426, #3997, #8173, #13704, #9513, #16785, #1456, #16692, #4086, #6987, #1287, #186, #2644, #1196, #6891, #5608, #9683, #15152, #16606, #10950, #12516, #5340, #9595, #3005, #10862, #13789, #4184, #15058, #6810, #13872, #16431, #4353, #101, #12336, #9864, #17900, #5695, #4268, #5431, #11210, #16513, #1367, #9770, #8430, #2734, #12420, #13968, #15419, #8256, #12254, #7, #11125, #2901, #12606, #15323, #1554, #6713, #7088, #11042, #15234, #5523, #2812, #8525, #17822, #8337, #3090, #3272, #6064, #3446, #10234, #17161, #8805, #4794, #15691, #7362, #11591, #1831, #8611, #11307, #4528 ) ),
 .UNSPECIFIED., .F., .F., .T. ) 
 B_SPLINE_SURFACE_WITH_KNOTS ( ( 2, 2 ),
 ( 3, 2, 2, 2, 2, 2, 2, 2, 2, 2, 2, 2, 2, 2, 2, 2, 2, 2, 2, 2, 2, 2, 2, 2, 2, 2, 2, 2, 2, 2, 2, 2, 2, 2, 2, 2, 2, 2, 2, 2, 2, 2, 2, 2, 2, 2, 2, 2, 2, 2, 2, 2, 2, 2, 2, 2, 2, 2, 2, 2, 2, 2, 2, 2, 2, 2, 2, 2, 2, 2, 2, 2, 2, 2, 2, 2, 2, 3 ),
 ( 0.000000000000000000, 1.000000000000000000 ),
 ( 0.000000000000000000, 0.01282051282051282007, 0.02564102564102564014, 0.03846153846153846367, 0.05128205128205128027, 0.06410256410256409687, 0.07692307692307692735, 0.08974358974358974395, 0.1025641025641025605, 0.1153846153846153910, 0.1282051282051281937, 0.1410256410256410242, 0.1538461538461538547, 0.1666666666666666574, 0.1794871794871794879, 0.1923076923076923184, 0.2051282051282051211, 0.2179487179487179516, 0.2307692307692307820, 0.2435897435897435848, 0.2564102564102563875, 0.2692307692307692180, 0.2820512820512820484, 0.2948717948717948789, 0.3076923076923077094, 0.3205128205128205399, 0.3333333333333333148, 0.3461538461538461453, 0.3589743589743589758, 0.3717948717948718063, 0.3846153846153846367, 0.3974358974358974117, 0.4102564102564102422, 0.4230769230769230727, 0.4358974358974359031, 0.4487179487179487336, 0.4615384615384615641, 0.4743589743589743390, 0.4871794871794871695, 0.5000000000000000000, 0.5128205128205127750, 0.5256410256410256610, 0.5384615384615384359, 0.5512820512820513219, 0.5641025641025640969, 0.5769230769230768718, 0.5897435897435897578, 0.6025641025641025328, 0.6153846153846154188, 0.6282051282051281937, 0.6410256410256410797, 0.6538461538461538547, 0.6666666666666666297, 0.6794871794871795156, 0.6923076923076922906, 0.7051282051282051766, 0.7179487179487179516, 0.7307692307692307265, 0.7435897435897436125, 0.7564102564102563875, 0.7692307692307692735, 0.7820512820512820484, 0.7948717948717948234, 0.8076923076923077094, 0.8205128205128204844, 0.8333333333333333703, 0.8461538461538461453, 0.8589743589743589203, 0.8717948717948718063, 0.8846153846153845812, 0.8974358974358974672, 0.9102564102564102422, 0.9230769230769231282, 0.9358974358974359031, 0.9487179487179486781, 0.9615384615384615641, 0.9690837477411259338, 0.9787745852185372186 ),
 .UNSPECIFIED. ) 
 GEOMETRIC_REPRESENTATION_ITEM ( )  RATIONAL_B_SPLINE_SURFACE ( (
 ( 1.000000000000000000, 0.8660254037844387076, 1.000000000000000000, 0.8660254037844387076, 1.000000000000000000, 0.8660254037844387076, 1.000000000000000000, 0.8660254037844387076, 1.000000000000000000, 0.8660254037844387076, 1.000000000000000000, 0.8660254037844387076, 1.000000000000000000, 0.8660254037844387076, 1.000000000000000000, 0.8660254037844387076, 1.000000000000000000, 0.8660254037844387076, 1.000000000000000000, 0.8660254037844387076, 1.000000000000000000, 0.8660254037844387076, 1.000000000000000000, 0.8660254037844387076, 1.000000000000000000, 0.8660254037844387076, 1.000000000000000000, 0.8660254037844387076, 1.000000000000000000, 0.8660254037844387076, 1.000000000000000000, 0.8660254037844387076, 1.000000000000000000, 0.8660254037844387076, 1.000000000000000000, 0.8660254037844387076, 1.000000000000000000, 0.8660254037844387076, 1.000000000000000000, 0.8660254037844387076, 1.000000000000000000, 0.8660254037844387076, 1.000000000000000000, 0.8660254037844387076, 1.000000000000000000, 0.8660254037844387076, 1.000000000000000000, 0.8660254037844387076, 1.000000000000000000, 0.8660254037844387076, 1.000000000000000000, 0.8660254037844387076, 1.000000000000000000, 0.8660254037844387076, 1.000000000000000000, 0.8660254037844387076, 1.000000000000000000, 0.8660254037844387076, 1.000000000000000000, 0.8660254037844387076, 1.000000000000000000, 0.8660254037844387076, 1.000000000000000000, 0.8660254037844387076, 1.000000000000000000, 0.8660254037844387076, 1.000000000000000000, 0.8660254037844387076, 1.000000000000000000, 0.8660254037844387076, 1.000000000000000000, 0.8660254037844387076, 1.000000000000000000, 0.8660254037844387076, 1.000000000000000000, 0.8660254037844387076, 1.000000000000000000, 0.8660254037844387076, 1.000000000000000000, 0.8660254037844387076, 1.000000000000000000, 0.8660254037844387076, 1.000000000000000000, 0.8660254037844387076, 1.000000000000000000, 0.8660254037844387076, 1.000000000000000000, 0.8660254037844387076, 1.000000000000000000, 0.8660254037844387076, 1.000000000000000000, 0.8660254037844387076, 1.000000000000000000, 0.8660254037844387076, 1.000000000000000000, 0.8660254037844387076, 1.000000000000000000, 0.8660254037844387076, 1.000000000000000000, 0.8660254037844387076, 1.000000000000000000, 0.8660254037844387076, 1.000000000000000000, 0.8660254037844387076, 1.000000000000000000, 0.8660254037844387076, 1.000000000000000000, 0.8660254037844387076, 1.000000000000000000, 0.8660254037844387076, 1.000000000000000000, 0.8660254037844387076, 1.000000000000000000, 0.8660254037844387076, 1.000000000000000000, 0.8660254037844387076, 1.000000000000000000, 0.8660254037844387076, 1.000000000000000000, 0.8660254037844387076, 1.000000000000000000, 0.8660254037844387076, 1.000000000000000000, 0.8660254037844387076, 1.000000000000000000, 0.8660254037844387076, 1.000000000000000000, 0.8660254037844387076, 1.000000000000000000, 0.8660254037844387076, 1.000000000000000000, 0.8660254037844387076, 1.000000000000000000, 0.8660254037844387076, 1.000000000000000000, 0.8660254037844387076, 1.000000000000000000, 0.8660254037844387076, 1.000000000000000000, 0.8660254037844387076, 1.000000000000000000, 0.8660254037844387076, 1.000000000000000000, 0.8660254037844387076, 1.000000000000000000, 0.8660254037844387076, 1.000000000000000000, 0.8660254037844387076, 1.000000000000000000, 0.8660254037844387076, 1.000000000000000000, 0.9211516195580409239, 0.9351128802560608744, 0.9351128802560608744, 0.9351128802560608744),
 ( 1.000000000000000000, 0.8660254037844387076, 1.000000000000000000, 0.8660254037844387076, 1.000000000000000000, 0.8660254037844387076, 1.000000000000000000, 0.8660254037844387076, 1.000000000000000000, 0.8660254037844387076, 1.000000000000000000, 0.8660254037844387076, 1.000000000000000000, 0.8660254037844387076, 1.000000000000000000, 0.8660254037844387076, 1.000000000000000000, 0.8660254037844387076, 1.000000000000000000, 0.8660254037844387076, 1.000000000000000000, 0.8660254037844387076, 1.000000000000000000, 0.8660254037844387076, 1.000000000000000000, 0.8660254037844387076, 1.000000000000000000, 0.8660254037844387076, 1.000000000000000000, 0.8660254037844387076, 1.000000000000000000, 0.8660254037844387076, 1.000000000000000000, 0.8660254037844387076, 1.000000000000000000, 0.8660254037844387076, 1.000000000000000000, 0.8660254037844387076, 1.000000000000000000, 0.8660254037844387076, 1.000000000000000000, 0.8660254037844387076, 1.000000000000000000, 0.8660254037844387076, 1.000000000000000000, 0.8660254037844387076, 1.000000000000000000, 0.8660254037844387076, 1.000000000000000000, 0.8660254037844387076, 1.000000000000000000, 0.8660254037844387076, 1.000000000000000000, 0.8660254037844387076, 1.000000000000000000, 0.8660254037844387076, 1.000000000000000000, 0.8660254037844387076, 1.000000000000000000, 0.8660254037844387076, 1.000000000000000000, 0.8660254037844387076, 1.000000000000000000, 0.8660254037844387076, 1.000000000000000000, 0.8660254037844387076, 1.000000000000000000, 0.8660254037844387076, 1.000000000000000000, 0.8660254037844387076, 1.000000000000000000, 0.8660254037844387076, 1.000000000000000000, 0.8660254037844387076, 1.000000000000000000, 0.8660254037844387076, 1.000000000000000000, 0.8660254037844387076, 1.000000000000000000, 0.8660254037844387076, 1.000000000000000000, 0.8660254037844387076, 1.000000000000000000, 0.8660254037844387076, 1.000000000000000000, 0.8660254037844387076, 1.000000000000000000, 0.8660254037844387076, 1.000000000000000000, 0.8660254037844387076, 1.000000000000000000, 0.8660254037844387076, 1.000000000000000000, 0.8660254037844387076, 1.000000000000000000, 0.8660254037844387076, 1.000000000000000000, 0.8660254037844387076, 1.000000000000000000, 0.8660254037844387076, 1.000000000000000000, 0.8660254037844387076, 1.000000000000000000, 0.8660254037844387076, 1.000000000000000000, 0.8660254037844387076, 1.000000000000000000, 0.8660254037844387076, 1.000000000000000000, 0.8660254037844387076, 1.000000000000000000, 0.8660254037844387076, 1.000000000000000000, 0.8660254037844387076, 1.000000000000000000, 0.8660254037844387076, 1.000000000000000000, 0.8660254037844387076, 1.000000000000000000, 0.8660254037844387076, 1.000000000000000000, 0.8660254037844387076, 1.000000000000000000, 0.8660254037844387076, 1.000000000000000000, 0.8660254037844387076, 1.000000000000000000, 0.8660254037844387076, 1.000000000000000000, 0.8660254037844387076, 1.000000000000000000, 0.8660254037844387076, 1.000000000000000000, 0.8660254037844387076, 1.000000000000000000, 0.8660254037844387076, 1.000000000000000000, 0.8660254037844387076, 1.000000000000000000, 0.8660254037844387076, 1.000000000000000000, 0.8660254037844387076, 1.000000000000000000, 0.8660254037844387076, 1.000000000000000000, 0.8660254037844387076, 1.000000000000000000, 0.8660254037844387076, 1.000000000000000000, 0.8660254037844387076, 1.000000000000000000, 0.9211516195580409239, 0.9351128802560608744, 0.9351128802560608744, 0.9351128802560608744) ) ) 
 REPRESENTATION_ITEM ( '' )  SURFACE ( )  );
#16301 = ORIENTED_EDGE ( 'NONE', *, *, #3605, .F. ) ;
#16302 = EDGE_CURVE ( 'NONE', #6794, #15658, #964, .T. ) ;
#16303 = CARTESIAN_POINT ( 'NONE',  ( 0.000000000000000000, 0.000000000000000000, -4.394516984716110741 ) ) ;
#16304 = CARTESIAN_POINT ( 'NONE',  ( 27.82847066025702887, -2.165988739474055791, 5.783357778048667797 ) ) ;
#16305 = CARTESIAN_POINT ( 'NONE',  ( 0.000000000000000000, 0.000000000000000000, 0.000000000000000000 ) ) ;
#16306 = CARTESIAN_POINT ( 'NONE',  ( 26.24062359194589078, -6.129313013101781671, 7.939653947423658487 ) ) ;
#16307 = CIRCLE ( 'NONE', #1247, 2.749999999999995559 ) ;
#16308 = CARTESIAN_POINT ( 'NONE',  ( 0.000000000000000000, 2.357898499370432166, -2.385244779468109755E-15 ) ) ;
#16309 = CARTESIAN_POINT ( 'NONE',  ( 31.11087420047036289, -5.742416513891037688, -3.283357778048667797 ) ) ;
#16310 = AXIS2_PLACEMENT_3D ( 'NONE', #16899, #7375, #12889 ) ;
#16311 = DIRECTION ( 'NONE',  ( 0.000000000000000000, 0.000000000000000000, -1.000000000000000000 ) ) ;
#16312 = CIRCLE ( 'NONE', #5554, 12.50000000000000000 ) ;
#16313 = CARTESIAN_POINT ( 'NONE',  ( 28.83304567166618781, -6.743756660494150346, 4.533357778048659803 ) ) ;
#16314 = VERTEX_POINT ( 'NONE', #13463 ) ;
#16315 = VERTEX_POINT ( 'NONE', #852 ) ;
#16316 = VERTEX_POINT ( 'NONE', #5018 ) ;
#16317 = ADVANCED_FACE ( 'NONE', ( #13271 ), #2407, .F. ) ;
#16318 = CARTESIAN_POINT ( 'NONE',  ( 30.75425665345519732, -2.450656702321377001, 6.861505862736165362 ) ) ;
#16319 = AXIS2_PLACEMENT_3D ( 'NONE', #11175, #13927, #15475 ) ;
#16320 = FACE_OUTER_BOUND ( 'NONE', #10656, .T. ) ;
#16321 = CARTESIAN_POINT ( 'NONE',  ( 29.56783163384821833, -3.220568019956291383, 3.627061608673666449 ) ) ;
#16322 = VERTEX_POINT ( 'NONE', #1039 ) ;
#16323 = PLANE ( 'NONE',  #6327 ) ;
#16324 = CARTESIAN_POINT ( 'NONE',  ( 32.69820532807177216, -4.097360875439379768, 8.283357778048662468 ) ) ;
#16325 = AXIS2_PLACEMENT_3D ( 'NONE', #12269, #14732, #7924 ) ;
#16326 = CARTESIAN_POINT ( 'NONE',  ( 25.93714794488954212, -2.393855775999666591, -5.783357778048658027 ) ) ;
#16327 = CARTESIAN_POINT ( 'NONE',  ( 28.89355063163679915, -2.047864499088824175, -5.783357778048658027 ) ) ;
#16328 = CARTESIAN_POINT ( 'NONE',  ( 28.52524344760924180, -2.419399995203538101, -7.033357778048658027 ) ) ;
#16329 = ORIENTED_EDGE ( 'NONE', *, *, #8106, .T. ) ;
#16330 = CARTESIAN_POINT ( 'NONE',  ( 33.21234388421201089, -5.489230917751459771, -8.283357778048662468 ) ) ;
#16331 = FACE_OUTER_BOUND ( 'NONE', #5592, .T. ) ;
#16332 = SHAPE_REPRESENTATION ( 'ceramic piston', ( #3575 ), #3784 ) ;
#16333 = CARTESIAN_POINT ( 'NONE',  ( 4.211140560182196957, -2.431303136016550237, -3.445885042887436800 ) ) ;
#16334 = CARTESIAN_POINT ( 'NONE',  ( 16.75000000000000000, -15.80031936969768935, 16.03574476417183803 ) ) ;
#16335 = FILL_AREA_STYLE ('',( #16414 ) ) ;
#16336 = ORIENTED_EDGE ( 'NONE', *, *, #12076, .T. ) ;
#16337 = CARTESIAN_POINT ( 'NONE',  ( 30.30787278169304244, -6.266260340387784566, -4.705209693361169343 ) ) ;
#16338 = CARTESIAN_POINT ( 'NONE',  ( 30.15443244188179150, -1.895953141405083864, -5.783357778048658915 ) ) ;
#16339 = ORIENTED_EDGE ( 'NONE', *, *, #17955, .T. ) ;
#16340 = DIRECTION ( 'NONE',  ( -0.1196152422706611984, 0.9928203230275510771, 0.000000000000000000 ) ) ;
#16341 = CIRCLE ( 'NONE', #14310, 5.000000000000000000 ) ;
#16342 = DIRECTION ( 'NONE',  ( 0.000000000000000000, 0.000000000000000000, 1.000000000000000000 ) ) ;
#16343 = AXIS2_PLACEMENT_3D ( 'NONE', #8879, #14605, #11949 ) ;
#16344 = ORIENTED_EDGE ( 'NONE', *, *, #4147, .T. ) ;
#16345 = VERTEX_POINT ( 'NONE', #11638 ) ;
#16346 = EDGE_CURVE ( 'NONE', #5903, #13433, #4747, .T. ) ;
#16347 = CARTESIAN_POINT ( 'NONE',  ( 32.02836186724004364, -4.178063784105134459, 3.627061608673664228 ) ) ;
#16348 = CARTESIAN_POINT ( 'NONE',  ( 28.76238721243587548, -5.825490297734302381, -3.627061608673667781 ) ) ;
#16349 = CARTESIAN_POINT ( 'NONE',  ( 0.000000000000000000, 0.000000000000000000, -2.000000000000000000 ) ) ;
#16350 = CARTESIAN_POINT ( 'NONE',  ( 28.44643833274707845, -2.428894455266221275, -7.033357778048658027 ) ) ;
#16351 = LINE ( 'NONE', #7989, #12171 ) ;
#16352 = LINE ( 'NONE', #3995, #51 ) ;
#16353 = AXIS2_PLACEMENT_3D ( 'NONE', #12932, #14590, #13207 ) ;
#16354 = EDGE_CURVE ( 'NONE', #2438, #13145, #3395, .T. ) ;
#16355 = CARTESIAN_POINT ( 'NONE',  ( 31.24221605398236790, -5.726592414339752857, -8.283357778048662468 ) ) ;
#16356 = CYLINDRICAL_SURFACE ( 'NONE', #3430, 10.50000000000000000 ) ;
#16357 = LINE ( 'NONE', #3835, #15984 ) ;
#16358 = DIRECTION ( 'NONE',  ( 0.000000000000000000, 0.000000000000000000, 1.000000000000000000 ) ) ;
#16359 = FACE_OUTER_BOUND ( 'NONE', #13021, .T. ) ;
#16360 = CARTESIAN_POINT ( 'NONE',  ( 26.39379627684682106, -4.856917663858078882, -3.283357778048664688 ) ) ;
#16361 = CARTESIAN_POINT ( 'NONE',  ( 33.19286683830256379, -2.783822866615540459, -7.939653947423660263 ) ) ;
#16362 = EDGE_CURVE ( 'NONE', #14027, #2784, #16424, .T. ) ;
#16363 = B_SPLINE_CURVE_WITH_KNOTS ( 'NONE', 3,
 ( #1575, #2100, #7623, #6249, #11771, #3535, #17061, #636, #15966, #15342, #12622, #4615, #4284, #203 ),
 .UNSPECIFIED., .F., .F.,
 ( 4, 2, 2, 2, 2, 2, 4 ),
 ( 0.000000000000000000, 0.004968481363098090076, 0.007452722044647132511, 0.009936962726196174947, 0.01490544408929426155, 0.01738968477084330486, 0.01987392545239234642 ),
 .UNSPECIFIED. ) ;
#16364 = CARTESIAN_POINT ( 'NONE',  ( -23.00000000000000000, -16.21813761408365195, -13.00000000000000355 ) ) ;
#16365 = ORIENTED_EDGE ( 'NONE', *, *, #12252, .F. ) ;
#16366 = CARTESIAN_POINT ( 'NONE',  ( -2.016448651773435938E-27, -20.49999999999999645, -6.000000000000000000 ) ) ;
#16367 = ORIENTED_EDGE ( 'NONE', *, *, #15285, .T. ) ;
#16368 = SURFACE_STYLE_USAGE ( .BOTH. , #5273 ) ;
#16369 = CARTESIAN_POINT ( 'NONE',  ( 31.02146712245815507, -5.553315781884258229, -7.939653947423662927 ) ) ;
#16370 = FACE_OUTER_BOUND ( 'NONE', #12346, .T. ) ;
#16371 = CARTESIAN_POINT ( 'NONE',  ( 26.15738093914773543, -4.885401043216321959, -8.283357778048662468 ) ) ;
#16372 = FACE_OUTER_BOUND ( 'NONE', #5531, .T. ) ;
#16373 = DIRECTION ( 'NONE',  ( 1.000000000000000000, 0.000000000000000000, 0.000000000000000000 ) ) ;
#16374 = CARTESIAN_POINT ( 'NONE',  ( 25.74134610602432360, -2.427642893298174620, -5.783357778048658027 ) ) ;
#16375 = PLANE ( 'NONE',  #8341 ) ;
#16376 = CARTESIAN_POINT ( 'NONE',  ( 30.49166216014303643, -4.363205751385915931, 3.283357778048664244 ) ) ;
#16377 = ORIENTED_EDGE ( 'NONE', *, *, #14376, .T. ) ;
#16378 = ADVANCED_FACE ( 'NONE', ( #9701 ), #10793, .F. ) ;
#16379 = CARTESIAN_POINT ( 'NONE',  ( 28.26310972651430120, -2.123820177930694442, 5.783357778048668685 ) ) ;
#16380 = CARTESIAN_POINT ( 'NONE',  ( -18.05564684537134568, -12.37312016356480449, 15.83930707548887895 ) ) ;
#16381 = CARTESIAN_POINT ( 'NONE',  ( 18.06124445020232727, -20.07065898529088344, 15.83842874644866505 ) ) ;
#16382 = VERTEX_POINT ( 'NONE', #1388 ) ;
#16383 = ORIENTED_EDGE ( 'NONE', *, *, #12255, .F. ) ;
#16384 = DIRECTION ( 'NONE',  ( 0.9928203230275510771, 0.1196152422706614205, 0.000000000000000000 ) ) ;
#16385 = ORIENTED_EDGE ( 'NONE', *, *, #10713, .T. ) ;
#16386 = VERTEX_POINT ( 'NONE', #17751 ) ;
#16387 = CARTESIAN_POINT ( 'NONE',  ( 33.95908713831673964, -3.945449517755637014, -5.783357778048663356 ) ) ;
#16388 = CARTESIAN_POINT ( 'NONE',  ( 30.78487334700428590, -1.819997462563214263, -5.783357778048658027 ) ) ;
#16389 = CARTESIAN_POINT ( 'NONE',  ( -3.999999999999998224, 0.000000000000000000, 0.000000000000000000 ) ) ;
#16390 = CARTESIAN_POINT ( 'NONE',  ( 26.35439372113758694, -4.861664893681965083, 3.627061608673664228 ) ) ;
#16391 = CARTESIAN_POINT ( 'NONE',  ( 29.60297508593253468, -5.724216059278466773, 3.627061608673662896 ) ) ;
#16392 = DIRECTION ( 'NONE',  ( 0.000000000000000000, 0.000000000000000000, 1.000000000000000000 ) ) ;
#16393 = CARTESIAN_POINT ( 'NONE',  ( 32.55256711014040150, -6.632986398338614364, 5.113484796970852564 ) ) ;
#16394 = CARTESIAN_POINT ( 'NONE',  ( 2.500000000000000000, 2.357898499370432166, -2.385244779468109755E-15 ) ) ;
#16395 = CARTESIAN_POINT ( 'NONE',  ( 28.09753128235661279, -6.832371619143005503, 7.033357778048657138 ) ) ;
#16396 = ORIENTED_EDGE ( 'NONE', *, *, #3693, .T. ) ;
#16397 = EDGE_CURVE ( 'NONE', #5110, #16590, #2667, .T. ) ;
#16398 = ORIENTED_EDGE ( 'NONE', *, *, #12361, .F. ) ;
#16399 = CARTESIAN_POINT ( 'NONE',  ( 30.67110321781257909, -3.087645581983020637, 3.627061608673666893 ) ) ;
#16400 = CARTESIAN_POINT ( 'NONE',  ( 27.55969062878875064, -7.234529412811931515, 5.783357778048657138 ) ) ;
#16401 = CARTESIAN_POINT ( 'NONE',  ( 30.41294626588012306, -6.253601060580800564, 4.705209693361159573 ) ) ;
#16402 = ORIENTED_EDGE ( 'NONE', *, *, #6758, .F. ) ;
#16403 =( BOUNDED_CURVE ( )  B_SPLINE_CURVE ( 3, ( #8500, #10114, #9841, #1531 ),
 .UNSPECIFIED., .F., .T. ) 
 B_SPLINE_CURVE_WITH_KNOTS ( ( 4, 4 ),
 ( 4.889642689481717319, 5.052230418047667371 ),
 .UNSPECIFIED. ) 
 CURVE ( )  GEOMETRIC_REPRESENTATION_ITEM ( )  RATIONAL_B_SPLINE_CURVE ( ( 1.000000000000000000, 0.9977983154653931042, 0.9977983154653931042, 1.000000000000000000 ) ) 
 REPRESENTATION_ITEM ( '' )  );
#16404 = DIRECTION ( 'NONE',  ( 0.9928203230275511881, 0.1196152422706614482, 0.000000000000000000 ) ) ;
#16405 = FACE_OUTER_BOUND ( 'NONE', #1475, .T. ) ;
#16406 = LINE ( 'NONE', #10498, #13661 ) ;
#16407 = PLANE ( 'NONE',  #951 ) ;
#16408 = CARTESIAN_POINT ( 'NONE',  ( 33.95908713831673964, -3.945449517755637903, 5.783357778048663356 ) ) ;
#16409 = ADVANCED_FACE ( 'NONE', ( #9532, #16447 ), #4016, .T. ) ;
#16410 = PLANE ( 'NONE',  #12265 ) ;
#16411 = DIRECTION ( 'NONE',  ( 0.9928203230275512992, 0.1196152422706610180, 4.006172263299093133E-17 ) ) ;
#16412 = CARTESIAN_POINT ( 'NONE',  ( 16.75000000000000000, -15.80031936969768935, -16.03574476417183803 ) ) ;
#16413 = CARTESIAN_POINT ( 'NONE',  ( 7.499998387031003411, -20.49508120620799900, -17.00000000000000000 ) ) ;
#16414 = FILL_AREA_STYLE_COLOUR ( '', #2077 ) ;
#16415 = EDGE_CURVE ( 'NONE', #16863, #9563, #9608, .T. ) ;
#16416 = CARTESIAN_POINT ( 'NONE',  ( 31.54230778485832332, -2.355712103769039611, -4.705209693361160461 ) ) ;
#16417 = CARTESIAN_POINT ( 'NONE',  ( 29.13014440709066832, -5.781182818409868140, -7.939653947423662927 ) ) ;
#16418 = DIRECTION ( 'NONE',  ( 0.1196152422706605323, -0.9928203230275512992, 0.000000000000000000 ) ) ;
#16419 = CARTESIAN_POINT ( 'NONE',  ( 31.63243098167119172, -2.771952051906466430, -8.283357778048660691 ) ) ;
#16420 = ORIENTED_EDGE ( 'NONE', *, *, #1761, .T. ) ;
#16421 = EDGE_LOOP ( 'NONE', ( #11802, #10289, #1068, #9730 ) ) ;
#16422 = CARTESIAN_POINT ( 'NONE',  ( 33.17547354829333983, -5.293800545841212291, 7.939653947423658487 ) ) ;
#16423 = CARTESIAN_POINT ( 'NONE',  ( 29.19137779418881351, -4.519864338893556877, -3.627061608673664672 ) ) ;
#16424 =( BOUNDED_CURVE ( )  B_SPLINE_CURVE ( 3, ( #15249, #17840, #10878, #6645 ),
 .UNSPECIFIED., .F., .T. ) 
 B_SPLINE_CURVE_WITH_KNOTS ( ( 4, 4 ),
 ( 1.514099494053832595, 1.567750514535811712 ),
 .UNSPECIFIED. ) 
 CURVE ( )  GEOMETRIC_REPRESENTATION_ITEM ( )  RATIONAL_B_SPLINE_CURVE ( ( 1.000000000000000000, 0.9997601450507493936, 0.9997601450507493936, 1.000000000000000000 ) ) 
 REPRESENTATION_ITEM ( '' )  );
#16425 = CARTESIAN_POINT ( 'NONE',  ( 32.26287188679368256, -2.695996373064596607, -8.283357778048660691 ) ) ;
#16426 = CARTESIAN_POINT ( 'NONE',  ( 10.27627944162880702, -4.200961894323389956, -3.000000000000000888 ) ) ;
#16427 = CARTESIAN_POINT ( 'NONE',  ( 28.56093688906631911, -4.595820017735426255, -3.627061608673664672 ) ) ;
#16428 = CARTESIAN_POINT ( 'NONE',  ( 32.60321786976872005, -6.626883982076972934, 5.783357778048664244 ) ) ;
#16429 = CARTESIAN_POINT ( 'NONE',  ( 33.95908713831674675, -3.945449517755636126, -5.783357778048663356 ) ) ;
#16430 = CARTESIAN_POINT ( 'NONE',  ( 3.538288549924106796, -15.34800872113743431, 13.00000000000000178 ) ) ;
#16431 = CARTESIAN_POINT ( 'NONE',  ( 28.78802868011566929, -7.476087111406434893, -5.783357778048669573 ) ) ;
#16432 = VERTEX_POINT ( 'NONE', #12440 ) ;
#16433 = EDGE_CURVE ( 'NONE', #14045, #11061, #7309, .T. ) ;
#16434 = DIRECTION ( 'NONE',  ( 0.000000000000000000, 0.000000000000000000, -1.000000000000000000 ) ) ;
#16435 = CARTESIAN_POINT ( 'NONE',  ( 28.19013153391124860, -7.158573733970061248, -5.783357778048657138 ) ) ;
#16436 = CARTESIAN_POINT ( 'NONE',  ( 0.000000000000000000, 0.000000000000000000, 0.000000000000000000 ) ) ;
#16437 = CARTESIAN_POINT ( 'NONE',  ( 45.00000000000000711, -16.03270077640482683, -0.5379818257722508434 ) ) ;
#16438 = AXIS2_PLACEMENT_3D ( 'NONE', #9892, #17923, #7113 ) ;
#16439 = CARTESIAN_POINT ( 'NONE',  ( 30.27725608814395386, -6.896919580145944195, -5.783357778048668685 ) ) ;
#16440 = EDGE_LOOP ( 'NONE', ( #17043, #600, #6191, #8903 ) ) ;
#16441 = LINE ( 'NONE', #2822, #13449 ) ;
#16442 = CARTESIAN_POINT ( 'NONE',  ( 26.01652455409633902, -4.902371455920928156, -5.783357778048663356 ) ) ;
#16443 = ORIENTED_EDGE ( 'NONE', *, *, #8234, .T. ) ;
#16444 =( NAMED_UNIT ( * ) PLANE_ANGLE_UNIT ( ) SI_UNIT ( $, .RADIAN. ) );
#16445 = VECTOR ( 'NONE', #13434, 1000.000000000000000 ) ;
#16446 = CARTESIAN_POINT ( 'NONE',  ( 31.24031073583692475, -4.273008382657478954, -3.627061608673664672 ) ) ;
#16447 = FACE_OUTER_BOUND ( 'NONE', #14275, .T. ) ;
#16448 = ORIENTED_EDGE ( 'NONE', *, *, #47, .F. ) ;
#16449 = ADVANCED_FACE ( 'NONE', ( #16278 ), #15078, .T. ) ;
#16450 = CARTESIAN_POINT ( 'NONE',  ( 26.34507017448785504, -7.770415366711231009, -5.783357778048669573 ) ) ;
#16451 = ADVANCED_FACE ( 'NONE', ( #16370, #8194 ), #3850, .F. ) ;
#16452 = CARTESIAN_POINT ( 'NONE',  ( 10.27627944162883544, 4.200961894323318013, -3.000000000000000888 ) ) ;
#16453 = CARTESIAN_POINT ( 'NONE',  ( 4.203935404774564510, 1.640788256319079208, -3.298453876328896861 ) ) ;
#16454 = CARTESIAN_POINT ( 'NONE',  ( 25.86833963875586306, -3.039313213345869791, -4.705209693361160461 ) ) ;
#16455 = CARTESIAN_POINT ( 'NONE',  ( 29.37220822929407760, -7.016156836349003001, 5.783357778048657138 ) ) ;
#16456 = VECTOR ( 'NONE', #2184, 1000.000000000000000 ) ;
#16457 = VECTOR ( 'NONE', #8716, 1000.000000000000000 ) ;
#16458 = CARTESIAN_POINT ( 'NONE',  ( 30.17635249042624679, -2.520282741259753045, 4.705209693361168455 ) ) ;
#16459 = CARTESIAN_POINT ( 'NONE',  ( -16.75000000000000355, -15.80559819018441381, 16.03574476417185934 ) ) ;
#16460 = CARTESIAN_POINT ( 'NONE',  ( 17.40734525178378078, -19.01589366988068974, 15.93907283187074775 ) ) ;
#16461 = ORIENTED_EDGE ( 'NONE', *, *, #6720, .T. ) ;
#16462 = DIRECTION ( 'NONE',  ( 1.000000000000000000, 0.000000000000000000, 0.000000000000000000 ) ) ;
#16463 = VECTOR ( 'NONE', #2200, 1000.000000000000000 ) ;
#16464 = LINE ( 'NONE', #16546, #1450 ) ;
#16465 = DIRECTION ( 'NONE',  ( 0.9928203230275510771, 0.1196152422706609902, 4.006172263299092517E-17 ) ) ;
#16466 = CARTESIAN_POINT ( 'NONE',  ( 31.55553118839817728, -4.235030543236534939, -7.939653947423662039 ) ) ;
#16467 = LINE ( 'NONE', #5297, #8645 ) ;
#16468 = DIRECTION ( 'NONE',  ( -1.000000000000000000, -1.224646799147353207E-16, 0.000000000000000000 ) ) ;
#16469 = DIRECTION ( 'NONE',  ( 0.000000000000000000, 0.000000000000000000, 1.000000000000000000 ) ) ;
#16470 = CARTESIAN_POINT ( 'NONE',  ( 29.94002636988270538, -4.429666970165102136, -8.283357778048662468 ) ) ;
#16471 = CARTESIAN_POINT ( 'NONE',  ( 28.35948656569675919, -3.366149737736551906, 7.939653947423664704 ) ) ;
#16472 = EDGE_CURVE ( 'NONE', #2403, #12037, #3933, .T. ) ;
#16473 = CARTESIAN_POINT ( 'NONE',  ( 26.01652455409633902, -4.902371455920926380, -5.783357778048663356 ) ) ;
#16474 = DIRECTION ( 'NONE',  ( 0.8243186046180107640, 0.5661261679878571984, 0.000000000000000000 ) ) ;
#16475 = FACE_OUTER_BOUND ( 'NONE', #6166, .T. ) ;
#16476 = EDGE_LOOP ( 'NONE', ( #5553, #2506 ) ) ;
#16477 = ADVANCED_FACE ( 'NONE', ( #6733 ), #28, .F. ) ;
#16478 = AXIS2_PLACEMENT_3D ( 'NONE', #6545, #8175, #1289 ) ;
#16479 = VERTEX_POINT ( 'NONE', #8097 ) ;
#16480 = CARTESIAN_POINT ( 'NONE',  ( 31.91006497951310550, -2.311404624444611589, 4.705209693361167567 ) ) ;
#16481 = LINE ( 'NONE', #11094, #4120 ) ;
#16482 = ORIENTED_EDGE ( 'NONE', *, *, #4753, .T. ) ;
#16483 = CARTESIAN_POINT ( 'NONE',  ( 28.51709679197738723, -3.347160818026084339, 7.939653947423662927 ) ) ;
#16484 =( NAMED_UNIT ( * ) PLANE_ANGLE_UNIT ( ) SI_UNIT ( $, .RADIAN. ) );
#16485 = CARTESIAN_POINT ( 'NONE',  ( -50.00000000000000000, -16.03270077640482683, -5.537981825772250843 ) ) ;
#16486 = DIRECTION ( 'NONE',  ( 0.000000000000000000, 0.000000000000000000, 1.000000000000000000 ) ) ;
#16487 = CARTESIAN_POINT ( 'NONE',  ( 26.00347982711925710, -2.723222710571018279, -7.033357778048658027 ) ) ;
#16488 = CARTESIAN_POINT ( 'NONE',  ( 28.84872679426759845, -7.079226011327149237, -6.453230759126474148 ) ) ;
#16489 = CARTESIAN_POINT ( 'NONE',  ( 31.38859741546781379, -7.162769935976271540, -5.783357778048669573 ) ) ;
#16490 = CARTESIAN_POINT ( 'NONE',  ( -1.499999999999999778, 9.380831519646861238, -2.000000000000000000 ) ) ;
#16491 = CARTESIAN_POINT ( 'NONE',  ( 42.32364987186199556, -2.937684895442014277, -5.783357778048662468 ) ) ;
#16492 = DIRECTION ( 'NONE',  ( 0.000000000000000000, 0.000000000000000000, -1.000000000000000000 ) ) ;
#16493 = CIRCLE ( 'NONE', #1172, 12.50000000000000000 ) ;
#16494 = ADVANCED_FACE ( 'NONE', ( #13632 ), #13803, .F. ) ;
#16495 = CARTESIAN_POINT ( 'NONE',  ( 31.69574812466957781, -6.726019302751734763, -5.783357778048669573 ) ) ;
#16496 = CARTESIAN_POINT ( 'NONE',  ( 29.56783163384821833, -3.220568019956291383, -7.939653947423660263 ) ) ;
#16497 = LINE ( 'NONE', #13516, #11814 ) ;
#16498 = DIRECTION ( 'NONE',  ( -1.000000000000000000, 0.000000000000000000, 0.000000000000000000 ) ) ;
#16499 = CIRCLE ( 'NONE', #10966, 5.500000000000000888 ) ;
#16500 = ADVANCED_FACE ( 'NONE', ( #5449, #10970 ), #16531, .T. ) ;
#16501 = ORIENTED_EDGE ( 'NONE', *, *, #15818, .T. ) ;
#16502 =( BOUNDED_CURVE ( )  B_SPLINE_CURVE ( 2, ( #3536, #13326, #15967, #17255, #6164, #726, #6250, #13232, #809 ),
 .UNSPECIFIED., .F., .T. ) 
 B_SPLINE_CURVE_WITH_KNOTS ( ( 3, 2, 2, 2, 3 ),
 ( 0.2500000000000000000, 0.2564102564102563875, 0.2692307692307692180, 0.2820512820512820484, 0.2884615384615384914 ),
 .UNSPECIFIED. ) 
 CURVE ( )  GEOMETRIC_REPRESENTATION_ITEM ( )  RATIONAL_B_SPLINE_CURVE ( ( 0.9330127018922194093, 0.9330127018922195203, 1.000000000000000000, 0.8660254037844387076, 1.000000000000000000, 0.8660254037844387076, 1.000000000000000000, 0.9330127018922190762, 0.9330127018922194093 ) ) 
 REPRESENTATION_ITEM ( '' )  );
#16503 = ORIENTED_EDGE ( 'NONE', *, *, #11669, .F. ) ;
#16504 = CARTESIAN_POINT ( 'NONE',  ( 32.75517961154501023, -5.344437665069116328, 3.627061608673662896 ) ) ;
#16505 = CARTESIAN_POINT ( 'NONE',  ( 29.62489513447700062, -6.348545659133139729, -6.861505862736166250 ) ) ;
#16506 = DIRECTION ( 'NONE',  ( 0.000000000000000000, 0.000000000000000000, -1.000000000000000000 ) ) ;
#16507 = DIRECTION ( 'NONE',  ( 0.000000000000000000, 1.000000000000000000, -0.000000000000000000 ) ) ;
#16508 = CARTESIAN_POINT ( 'NONE',  ( 27.72904566057427189, -3.442105416578422172, -3.627061608673662896 ) ) ;
#16509 = FACE_OUTER_BOUND ( 'NONE', #4391, .T. ) ;
#16510 = DIRECTION ( 'NONE',  ( 0.000000000000000000, 0.000000000000000000, 1.000000000000000000 ) ) ;
#16511 = B_SPLINE_CURVE_WITH_KNOTS ( 'NONE', 3,
 ( #2137, #7656, #759, #14812, #9358, #10698 ),
 .UNSPECIFIED., .F., .F.,
 ( 4, 2, 4 ),
 ( 0.002365888236227992047, 0.003551327329835083247, 0.004736766423442174447 ),
 .UNSPECIFIED. ) ;
#16512 = DIRECTION ( 'NONE',  ( -1.000000000000000000, 0.000000000000000000, 0.000000000000000000 ) ) ;
#16513 = CARTESIAN_POINT ( 'NONE',  ( 28.09001152836989235, -6.106370808549102414, -8.283357778048662468 ) ) ;
#16514 = ORIENTED_EDGE ( 'NONE', *, *, #985, .T. ) ;
#16515 = CARTESIAN_POINT ( 'NONE',  ( 4.000000000000000000, -2.309401076758510918, -3.133295621305383083 ) ) ;
#16516 = DIRECTION ( 'NONE',  ( 0.000000000000000000, 1.000000000000000000, -1.103561164596346103E-15 ) ) ;
#16517 = CYLINDRICAL_SURFACE ( 'NONE', #14977, 1.000000000000000000 ) ;
#16518 = DIRECTION ( 'NONE',  ( -1.000000000000000000, 0.000000000000000000, 0.000000000000000000 ) ) ;
#16519 = CARTESIAN_POINT ( 'NONE',  ( -3.540000644887186798, -2.810673041920830784, -3.302142222888937884 ) ) ;
#16520 = CARTESIAN_POINT ( 'NONE',  ( 28.13194630731337753, -5.901445976576172647, -3.627061608673667781 ) ) ;
#16521 =( BOUNDED_CURVE ( )  B_SPLINE_CURVE ( 2, ( #9963, #9870, #5976, #1464, #14251, #384, #3010, #4453, #5891 ),
 .UNSPECIFIED., .F., .T. ) 
 B_SPLINE_CURVE_WITH_KNOTS ( ( 3, 2, 2, 2, 3 ),
 ( 0.6730769230769231282, 0.6794871794871795156, 0.6923076923076922906, 0.7051282051282051766, 0.7115384615384615641 ),
 .UNSPECIFIED. ) 
 CURVE ( )  GEOMETRIC_REPRESENTATION_ITEM ( )  RATIONAL_B_SPLINE_CURVE ( ( 0.9330127018922192983, 0.9330127018922198534, 1.000000000000000000, 0.8660254037844387076, 1.000000000000000000, 0.8660254037844387076, 1.000000000000000000, 0.9330127018922194093, 0.9330127018922194093 ) ) 
 REPRESENTATION_ITEM ( '' )  );
#16522 = VECTOR ( 'NONE', #2260, 1000.000000000000000 ) ;
#16523 = DIRECTION ( 'NONE',  ( -0.000000000000000000, -0.000000000000000000, 1.000000000000000000 ) ) ;
#16524 = CARTESIAN_POINT ( 'NONE',  ( 30.60493568430522160, -6.867637522466304212, -5.113484796970860558 ) ) ;
#16525 = EDGE_CURVE ( 'NONE', #6659, #14281, #8271, .T. ) ;
#16526 = ORIENTED_EDGE ( 'NONE', *, *, #11293, .T. ) ;
#16527 = CARTESIAN_POINT ( 'NONE',  ( -27.94356719068602146, -12.38857420186734970, -13.73436385264702153 ) ) ;
#16528 = ORIENTED_EDGE ( 'NONE', *, *, #15110, .T. ) ;
#16529 = CARTESIAN_POINT ( 'NONE',  ( 29.03376756790819613, -4.538853258604016006, -7.939653947423662039 ) ) ;
#16530 =( GEOMETRIC_REPRESENTATION_CONTEXT ( 3 ) GLOBAL_UNCERTAINTY_ASSIGNED_CONTEXT ( ( #15690 ) ) GLOBAL_UNIT_ASSIGNED_CONTEXT ( ( #14317, #1900, #12760 ) ) REPRESENTATION_CONTEXT ( 'NONE', 'WORKASPACE' ) );
#16531 = PLANE ( 'NONE',  #14553 ) ;
#16532 = CARTESIAN_POINT ( 'NONE',  ( 27.57216386142120257, -6.895668018177890879, -7.033357778048666908 ) ) ;
#16533 = EDGE_CURVE ( 'NONE', #6357, #131, #5723, .T. ) ;
#16534 = CARTESIAN_POINT ( 'NONE',  ( 2.500000000000000000, -2.357898499370431722, 2.818925648462311528E-15 ) ) ;
#16535 = DIRECTION ( 'NONE',  ( 1.000000000000000000, 0.000000000000000000, 0.000000000000000000 ) ) ;
#16536 = AXIS2_PLACEMENT_3D ( 'NONE', #10590, #13432, #5155 ) ;
#16537 = CARTESIAN_POINT ( 'NONE',  ( 26.39370705969127684, -2.976016814310973313, -6.861505862736158257 ) ) ;
#16538 = ORIENTED_EDGE ( 'NONE', *, *, #9524, .F. ) ;
#16539 = DIRECTION ( 'NONE',  ( 0.9928203230275512992, 0.1196152422706610041, 9.614813431917824012E-17 ) ) ;
#16540 = ADVANCED_FACE ( 'NONE', ( #4706 ), #17254, .T. ) ;
#16541 = DIRECTION ( 'NONE',  ( -0.000000000000000000, -0.000000000000000000, 1.000000000000000000 ) ) ;
#16542 = DIRECTION ( 'NONE',  ( 0.9928203230275512992, 0.1196152422706610041, 9.614813431917824012E-17 ) ) ;
#16543 = DIRECTION ( 'NONE',  ( -0.000000000000000000, -0.000000000000000000, -1.000000000000000000 ) ) ;
#16544 = ORIENTED_EDGE ( 'NONE', *, *, #4540, .T. ) ;
#16545 = ORIENTED_EDGE ( 'NONE', *, *, #6251, .F. ) ;
#16546 = CARTESIAN_POINT ( 'NONE',  ( 39.61846472826311327, -7.045996035215874365, -5.783357778048665132 ) ) ;
#16547 = ORIENTED_EDGE ( 'NONE', *, *, #5941, .T. ) ;
#16548 = DIRECTION ( 'NONE',  ( 0.9928203230275512992, 0.1196152422706610180, 4.006172263299093133E-17 ) ) ;
#16549 = CARTESIAN_POINT ( 'NONE',  ( 30.39102621733566423, -5.629271460726126719, -7.939653947423664704 ) ) ;
#16550 = VECTOR ( 'NONE', #10411, 1000.000000000000114 ) ;
#16551 = AXIS2_PLACEMENT_3D ( 'NONE', #9594, #13525, #15150 ) ;
#16552 = FACE_OUTER_BOUND ( 'NONE', #5682, .T. ) ;
#16553 = CARTESIAN_POINT ( 'NONE',  ( 29.74110826630371207, -2.999819088432076786, 3.283357778048666464 ) ) ;
#16554 = DIRECTION ( 'NONE',  ( 1.000000000000000000, 0.000000000000000000, 0.000000000000000000 ) ) ;
#16555 = CARTESIAN_POINT ( 'NONE',  ( -25.11802603177690330, -16.03270077640482683, -0.5379818257722508434 ) ) ;
#16556 = CARTESIAN_POINT ( 'NONE',  ( 30.27725608814395031, -6.896919580145944195, 5.783357778048658027 ) ) ;
#16557 = CYLINDRICAL_SURFACE ( 'NONE', #61, 2.500000000000001776 ) ;
#16558 = DIRECTION ( 'NONE',  ( 1.000000000000000000, 0.000000000000000000, 0.000000000000000000 ) ) ;
#16559 = AXIS2_PLACEMENT_3D ( 'NONE', #2366, #10840, #2615 ) ;
#16560 = CARTESIAN_POINT ( 'NONE',  ( 33.43363050022580296, -2.127845067243429256, 6.861505862736166250 ) ) ;
#16561 = VERTEX_POINT ( 'NONE', #5966 ) ;
#16562 = ORIENTED_EDGE ( 'NONE', *, *, #17240, .F. ) ;
#16563 = ORIENTED_EDGE ( 'NONE', *, *, #4582, .T. ) ;
#16564 = CIRCLE ( 'NONE', #13388, 2.540000000000001368 ) ;
#16565 = AXIS2_PLACEMENT_3D ( 'NONE', #16436, #8437, #14971 ) ;
#16566 = ORIENTED_EDGE ( 'NONE', *, *, #11645, .F. ) ;
#16567 = EDGE_CURVE ( 'NONE', #2813, #12087, #16363, .T. ) ;
#16568 = CARTESIAN_POINT ( 'NONE',  ( 27.75549246765397271, -7.200742295513423485, 5.783357778048658027 ) ) ;
#16569 = LINE ( 'NONE', #12217, #12223 ) ;
#16570 = ORIENTED_EDGE ( 'NONE', *, *, #8693, .T. ) ;
#16571 = EDGE_LOOP ( 'NONE', ( #3756, #15934 ) ) ;
#16572 = LINE ( 'NONE', #17956, #7500 ) ;
#16573 = CARTESIAN_POINT ( 'NONE',  ( 38.97925773053390941, -7.992821573592764572, -5.783357778048662468 ) ) ;
#16574 = CARTESIAN_POINT ( 'NONE',  ( 33.53059316159333036, -1.478995586096186532, -5.113484796970854340 ) ) ;
#16576 = VECTOR ( 'NONE', #6200, 1000.000000000000000 ) ;
#16575 = CARTESIAN_POINT ( 'NONE',  ( 27.02867472334902033, -6.034368414549446058, -3.627061608673668225 ) ) ;
#16577 = CARTESIAN_POINT ( 'NONE',  ( 29.95125523467787332, -2.974500528818129652, 8.283357778048666020 ) ) ;
#16578 = CARTESIAN_POINT ( 'NONE',  ( 29.18947247604337392, -3.066280307211263878, -8.283357778048658915 ) ) ;
#16579 = FACE_OUTER_BOUND ( 'NONE', #9370, .T. ) ;
#16580 = CARTESIAN_POINT ( 'NONE',  ( 3.511755186886750479, -2.826662030176377627, -3.297382984111582260 ) ) ;
#16581 = CARTESIAN_POINT ( 'NONE',  ( 33.95908713831673964, -3.945449517755648561, 5.783357778048663356 ) ) ;
#16582 = EDGE_CURVE ( 'NONE', #3948, #17429, #1919, .T. ) ;
#16583 = CIRCLE ( 'NONE', #15429, 10.50000000000000000 ) ;
#16584 = ORIENTED_EDGE ( 'NONE', *, *, #826, .F. ) ;
#16585 = CIRCLE ( 'NONE', #1519, 4.250000000000000000 ) ;
#16586 = CARTESIAN_POINT ( 'NONE',  ( 27.65458886993626564, -2.824105456627233224, -6.861505862736158257 ) ) ;
#16587 = CARTESIAN_POINT ( 'NONE',  ( 30.28142597461332741, -2.507623461452779701, -4.705209693361160461 ) ) ;
#16588 = CARTESIAN_POINT ( 'NONE',  ( 33.40745134805642635, -4.011910736534825439, 8.283357778048662468 ) ) ;
#16589 = DIRECTION ( 'NONE',  ( 0.9928203230275512992, 0.1196152422706587698, 0.000000000000000000 ) ) ;
#16590 = VERTEX_POINT ( 'NONE', #8454 ) ;
#16591 = ORIENTED_EDGE ( 'NONE', *, *, #15420, .T. ) ;
#16592 = CIRCLE ( 'NONE', #9334, 6.000000000000000888 ) ;
#16593 = ORIENTED_EDGE ( 'NONE', *, *, #3942, .F. ) ;
#16594 = DIRECTION ( 'NONE',  ( 0.9928203230275510771, 0.1196152422706609902, 4.006172263299092517E-17 ) ) ;
#16595 = CIRCLE ( 'NONE', #8784, 4.000000000000000000 ) ;
#16596 = CARTESIAN_POINT ( 'NONE',  ( 28.24571643650507369, -4.633797857156355171, -7.939653947423662039 ) ) ;
#16597 = DIRECTION ( 'NONE',  ( 0.000000000000000000, 0.000000000000000000, -1.000000000000000000 ) ) ;
#16598 = EDGE_CURVE ( 'NONE', #6324, #12037, #11324, .T. ) ;
#16599 = DIRECTION ( 'NONE',  ( 0.1196152422706608515, -0.9928203230275510771, 4.694733121053619507E-17 ) ) ;
#16600 = CARTESIAN_POINT ( 'NONE',  ( 1.499999999999999334, -5.809475019311126864, -3.000000000000000000 ) ) ;
#16601 = CARTESIAN_POINT ( 'NONE',  ( 28.24571643650507369, -4.633797857156355171, -7.939653947423662039 ) ) ;
#16602 = CARTESIAN_POINT ( 'NONE',  ( 32.32036211097666012, -1.624804527518282748, 5.783357778048663356 ) ) ;
#16603 = CARTESIAN_POINT ( 'NONE',  ( 0.2500000000000002220, 5.204748896376250699E-16, -4.250000000000000000 ) ) ;
#16604 = FACE_OUTER_BOUND ( 'NONE', #7414, .T. ) ;
#16605 = AXIS2_PLACEMENT_3D ( 'NONE', #15939, #6315, #17230 ) ;
#16606 = CARTESIAN_POINT ( 'NONE',  ( 29.41846958523816724, -7.400131432564565515, -5.783357778048669573 ) ) ;
#16607 = EDGE_CURVE ( 'NONE', #9975, #2513, #15165, .T. ) ;
#16608 = EDGE_CURVE ( 'NONE', #7736, #10032, #7918, .T. ) ;
#16609 = CARTESIAN_POINT ( 'NONE',  ( 29.99682221560115991, -1.914942061115552541, -5.783357778048658027 ) ) ;
#16610 = DIRECTION ( 'NONE',  ( -0.1414213562373112243, -0.9899494936611663576, 0.000000000000000000 ) ) ;
#16611 = CARTESIAN_POINT ( 'NONE',  ( 26.01652455409633902, -4.902371455920926380, -5.783357778048663356 ) ) ;
#16612 =( BOUNDED_SURFACE ( )  B_SPLINE_SURFACE ( 3, 2, ( 
 ( #17845, #6830, #15083 ),
 ( #11236, #1486, #13893 ),
 ( #4288, #2666, #9796 ),
 ( #5630, #5364, #16814 ),
 ( #8362, #4378, #16453 ),
 ( #12627, #4114, #12355 ) ),
 .UNSPECIFIED., .F., .F., .T. ) 
 B_SPLINE_SURFACE_WITH_KNOTS ( ( 4, 2, 4 ),
 ( 3, 3 ),
 ( 0.02018219363417822834, 0.02264238182714342976, 0.02510257002010863117 ),
 ( 0.000000000000000000, 1.000000000000000000 ),
 .UNSPECIFIED. ) 
 GEOMETRIC_REPRESENTATION_ITEM ( )  RATIONAL_B_SPLINE_SURFACE ( (
 ( 1.000000000000000000, 0.8047781633350724606, 1.000000000000000000),
 ( 1.000000000000000000, 0.8123767859461582530, 1.000000000000000000),
 ( 1.000000000000000000, 0.8190657615682832571, 1.000000000000000000),
 ( 1.000000000000000000, 0.8192365618914938530, 1.000000000000000000),
 ( 1.000000000000000000, 0.8126137554627823611, 1.000000000000000000),
 ( 1.000000000000000000, 0.8047712275319379716, 1.000000000000000000) ) ) 
 REPRESENTATION_ITEM ( '' )  SURFACE ( )  );
#16613 = CARTESIAN_POINT ( 'NONE',  ( 0.1756478951291680912, -4.720212513052437941, -3.169390900447856652 ) ) ;
#16614 = CARTESIAN_POINT ( 'NONE',  ( 30.23341599105502908, -5.648260380436596506, -7.939653947423662927 ) ) ;
#16615 = ORIENTED_EDGE ( 'NONE', *, *, #13004, .F. ) ;
#16616 = EDGE_LOOP ( 'NONE', ( #9947, #13480, #8510, #17948 ) ) ;
#16617 = DIRECTION ( 'NONE',  ( 1.000000000000000000, 0.000000000000000000, 0.000000000000000000 ) ) ;
#16618 = DIRECTION ( 'NONE',  ( 0.000000000000000000, -1.000000000000000000, 0.000000000000000000 ) ) ;
#16619 = CIRCLE ( 'NONE', #17809, 6.249999999999998224 ) ;
#16620 = CARTESIAN_POINT ( 'NONE',  ( -20.00000000000000355, 7.999999999999996447, -6.000000000000000000 ) ) ;
#16621 = ORIENTED_EDGE ( 'NONE', *, *, #3003, .T. ) ;
#16622 = CARTESIAN_POINT ( 'NONE',  ( 28.71854711534694715, -4.576831098024959132, -3.627061608673664672 ) ) ;
#16623 = CARTESIAN_POINT ( 'NONE',  ( 23.00000000000000000, -16.21813761408365195, 13.00000000000000178 ) ) ;
#16624 = EDGE_CURVE ( 'NONE', #4518, #11059, #4881, .T. ) ;
#16625 = ORIENTED_EDGE ( 'NONE', *, *, #16868, .T. ) ;
#16626 = CARTESIAN_POINT ( 'NONE',  ( 29.36638131047866196, -1.990897739957422807, -5.783357778048658027 ) ) ;
#16627 = LINE ( 'NONE', #10973, #3466 ) ;
#16628 = CARTESIAN_POINT ( 'NONE',  ( 32.14656953781143756, -4.163822094218565972, 8.283357778048662468 ) ) ;
#16629 = CARTESIAN_POINT ( 'NONE',  ( 28.41655006632555569, -6.494127376913395366, -4.705209693361169343 ) ) ;
#16630 = EDGE_CURVE ( 'NONE', #13349, #6877, #12852, .T. ) ;
#16631 = VERTEX_POINT ( 'NONE', #2921 ) ;
#16632 = CARTESIAN_POINT ( 'NONE',  ( 22.22189723075623036, -22.43265299876153662, -15.08700452545048343 ) ) ;
#16633 = ORIENTED_EDGE ( 'NONE', *, *, #2225, .T. ) ;
#16634 = CARTESIAN_POINT ( 'NONE',  ( 26.82722439997946395, -4.804698134550569044, 7.939653947423662039 ) ) ;
#16635 = CYLINDRICAL_SURFACE ( 'NONE', #13342, 13.00000000000000178 ) ;
#16636 = DIRECTION ( 'NONE',  ( -0.000000000000000000, -1.000000000000000000, -0.000000000000000000 ) ) ;
#16637 = EDGE_CURVE ( 'NONE', #13069, #5422, #16341, .T. ) ;
#16638 = VERTEX_POINT ( 'NONE', #13992 ) ;
#16639 = CARTESIAN_POINT ( 'NONE',  ( 28.53771668024168662, -2.080538600569502794, 5.783357778048667797 ) ) ;
#16640 = VERTEX_POINT ( 'NONE', #7108 ) ;
#16641 = DIRECTION ( 'NONE',  ( 1.000000000000000000, -1.734723475976805517E-15, 0.000000000000000000 ) ) ;
#16642 = VERTEX_POINT ( 'NONE', #11492 ) ;
#16643 = FACE_OUTER_BOUND ( 'NONE', #16208, .T. ) ;
#16644 = CARTESIAN_POINT ( 'NONE',  ( 26.51200394741821498, -4.842675973971495296, -7.939653947423662039 ) ) ;
#16645 = ORIENTED_EDGE ( 'NONE', *, *, #5941, .F. ) ;
#16646 = CARTESIAN_POINT ( 'NONE',  ( -4.000000000000000000, -1.942223658245630480, -0.3516579909967653128 ) ) ;
#16647 = CARTESIAN_POINT ( 'NONE',  ( 27.90727577511918867, -2.156494279411373061, -5.783357778048670461 ) ) ;
#16648 = CARTESIAN_POINT ( 'NONE',  ( 0.000000000000000000, 0.000000000000000000, 0.000000000000000000 ) ) ;
#16649 = CARTESIAN_POINT ( 'NONE',  ( 31.26353094466156080, -6.788289799823394866, -5.783357778048663356 ) ) ;
#16650 = CARTESIAN_POINT ( 'NONE',  ( 28.23249303296521617, -2.754479417688857179, 6.861505862736165362 ) ) ;
#16651 = EDGE_CURVE ( 'NONE', #16638, #4798, #2193, .T. ) ;
#16652 = DIRECTION ( 'NONE',  ( 1.000000000000000000, 0.000000000000000000, 0.000000000000000000 ) ) ;
#16653 = DIRECTION ( 'NONE',  ( 0.000000000000000000, 0.000000000000000000, 1.000000000000000000 ) ) ;
#16654 = CARTESIAN_POINT ( 'NONE',  ( -2.016448651773435938E-27, -20.49999999999999645, 13.00000000000000355 ) ) ;
#16655 = VERTEX_POINT ( 'NONE', #12133 ) ;
#16656 = ORIENTED_EDGE ( 'NONE', *, *, #11645, .T. ) ;
#16657 = EDGE_CURVE ( 'NONE', #11061, #133, #8497, .T. ) ;
#16658 = CARTESIAN_POINT ( 'NONE',  ( 27.12505156253147476, -7.276697974355294640, 5.783357778048658027 ) ) ;
#16659 = CARTESIAN_POINT ( 'NONE',  ( 28.84872679426759845, -7.079226011327149237, -6.453230759126474148 ) ) ;
#16660 = EDGE_CURVE ( 'NONE', #225, #2070, #10522, .T. ) ;
#16661 = ORIENTED_EDGE ( 'NONE', *, *, #5761, .T. ) ;
#16662 = CARTESIAN_POINT ( 'NONE',  ( 26.63030083514515312, -6.709335133632020387, 4.705209693361159573 ) ) ;
#16663 = ORIENTED_EDGE ( 'NONE', *, *, #1662, .F. ) ;
#16664 = EDGE_LOOP ( 'NONE', ( #7148, #5482, #9545, #11458, #7944 ) ) ;
#16665 = PRODUCT_DEFINITION ( 'UNKNOWN', '', #10334, #1921 ) ;
#16666 = DIRECTION ( 'NONE',  ( -0.1196152422706621005, 0.9928203230275509661, -0.000000000000000000 ) ) ;
#16667 = CARTESIAN_POINT ( 'NONE',  ( 33.60446413004628141, -3.988174587000466342, -3.627061608673664672 ) ) ;
#16668 = PLANE ( 'NONE',  #14545 ) ;
#16669 = CARTESIAN_POINT ( 'NONE',  ( 27.89118264539014547, -6.557423775948280742, -6.861505862736167138 ) ) ;
#16670 = CARTESIAN_POINT ( 'NONE',  ( -15.92260893619738837, -28.39189527176317540, 6.000000000000000000 ) ) ;
#16671 = CARTESIAN_POINT ( 'NONE',  ( 28.63031693179632242, -2.406740715396564756, -4.533357778048659803 ) ) ;
#16672 = CARTESIAN_POINT ( 'NONE',  ( 32.49625839967270480, -6.639770485940693412, -5.113484796970860558 ) ) ;
#16673 = DIRECTION ( 'NONE',  ( -0.1196152422706599633, 0.9928203230275514102, 0.000000000000000000 ) ) ;
#16674 = CARTESIAN_POINT ( 'NONE',  ( 35.77680296528374271, -19.03270077640482683, -10.53798182577225084 ) ) ;
#16675 = CARTESIAN_POINT ( 'NONE',  ( 29.36638131047866196, -1.990897739957422807, -5.783357778048658027 ) ) ;
#16676 = EDGE_CURVE ( 'NONE', #3230, #13090, #16619, .T. ) ;
#16677 = ADVANCED_FACE ( 'NONE', ( #7705, #10503 ), #16410, .T. ) ;
#16678 = CARTESIAN_POINT ( 'NONE',  ( 27.77288575766320378, -4.690764616287755651, -7.939653947423662039 ) ) ;
#16679 = DIRECTION ( 'NONE',  ( -0.1196152422706621143, 0.9928203230275509661, 0.000000000000000000 ) ) ;
#16680 = ORIENTED_EDGE ( 'NONE', *, *, #14916, .F. ) ;
#16681 = VERTEX_POINT ( 'NONE', #3633 ) ;
#16682 = EDGE_LOOP ( 'NONE', ( #16116, #16329, #6378, #15597 ) ) ;
#16683 = CARTESIAN_POINT ( 'NONE',  ( 30.15026255541241440, -6.285249260098253465, 6.861505862736158257 ) ) ;
#16684 = CARTESIAN_POINT ( 'NONE',  ( 26.35439372113758694, -4.861664893681965083, -7.939653947423662039 ) ) ;
#16685 = CARTESIAN_POINT ( 'NONE',  ( 3.199999999999999289, 0.000000000000000000, 2.399999999999999467 ) ) ;
#16686 = LINE ( 'NONE', #11203, #15332 ) ;
#16687 = CARTESIAN_POINT ( 'NONE',  ( 29.21955148510287614, -5.970283550416647600, -3.283357778048667797 ) ) ;
#16688 = CARTESIAN_POINT ( 'NONE',  ( 27.75549246765397271, -7.200742295513423485, -5.783357778048668685 ) ) ;
#16689 = CARTESIAN_POINT ( 'NONE',  ( 31.05948030073166066, -1.776715885202022394, -5.783357778048662468 ) ) ;
#16690 = CARTESIAN_POINT ( 'NONE',  ( 0.000000000000000000, 0.000000000000000000, 6.000000000000000000 ) ) ;
#16691 = CARTESIAN_POINT ( 'NONE',  ( 20.00000000000000000, 7.999999999999996447, -6.000000000000000000 ) ) ;
#16692 = CARTESIAN_POINT ( 'NONE',  ( 29.91004888286193619, -6.613999042680076990, -4.533357778048668685 ) ) ;
#16693 = CARTESIAN_POINT ( 'NONE',  ( 31.28415083292585663, -5.521667582366822202, -3.627061608673667781 ) ) ;
#16694 =( NAMED_UNIT ( * ) SI_UNIT ( $, .STERADIAN. ) SOLID_ANGLE_UNIT ( ) );
#16695 = CARTESIAN_POINT ( 'NONE',  ( 26.55511561737958814, -2.656761491791831187, -7.033357778048658027 ) ) ;
#16696 = DIRECTION ( 'NONE',  ( -1.000000000000000000, 0.000000000000000000, 0.000000000000000000 ) ) ;
#16697 = CARTESIAN_POINT ( 'NONE',  ( 42.32364987186199556, -2.937684895442014277, -5.783357778048662468 ) ) ;
#16698 = EDGE_CURVE ( 'NONE', #6479, #7654, #6691, .T. ) ;
#16699 = ORIENTED_EDGE ( 'NONE', *, *, #9447, .F. ) ;
#16700 = CARTESIAN_POINT ( 'NONE',  ( 30.33776104811456165, -2.201027418740610919, 4.533357778048667797 ) ) ;
#16701 = CARTESIAN_POINT ( 'NONE',  ( 27.47505859511117521, -2.218764776483033163, -5.783357778048658915 ) ) ;
#16702 = ORIENTED_EDGE ( 'NONE', *, *, #9180, .F. ) ;
#16703 = VERTEX_POINT ( 'NONE', #17712 ) ;
#16704 = ADVANCED_FACE ( 'NONE', ( #14694 ), #5865, .T. ) ;
#16705 = CARTESIAN_POINT ( 'NONE',  ( 26.01652455409633902, -4.902371455920926380, -5.783357778048663356 ) ) ;
#16706 = CARTESIAN_POINT ( 'NONE',  ( 7.499998387031003411, -20.49508120620799900, 12.00000000000000000 ) ) ;
#16707 = ORIENTED_EDGE ( 'NONE', *, *, #10821, .F. ) ;
#16708 = DIRECTION ( 'NONE',  ( 0.000000000000000000, 0.000000000000000000, 1.000000000000000000 ) ) ;
#16709 = ORIENTED_EDGE ( 'NONE', *, *, #10028, .T. ) ;
#16710 = CARTESIAN_POINT ( 'NONE',  ( 31.41531425212677675, -1.744041783721344219, -5.783357778048658915 ) ) ;
#16711 = DIRECTION ( 'NONE',  ( 0.000000000000000000, 0.000000000000000000, 1.000000000000000000 ) ) ;
#16712 = VERTEX_POINT ( 'NONE', #3325 ) ;
#16713 = VECTOR ( 'NONE', #576, 1000.000000000000114 ) ;
#16714 = CARTESIAN_POINT ( 'NONE',  ( 30.01874226414561875, -2.539271660970221944, -6.861505862736159145 ) ) ;
#16715 = DIRECTION ( 'NONE',  ( -1.000000000000000000, -0.000000000000000000, -0.000000000000000000 ) ) ;
#16716 = DIRECTION ( 'NONE',  ( -1.000000000000000000, 0.000000000000000000, 0.000000000000000000 ) ) ;
#16717 = ORIENTED_EDGE ( 'NONE', *, *, #16608, .F. ) ;
#16718 = CARTESIAN_POINT ( 'NONE',  ( 33.20111501597313719, -6.944397359513344803, -5.783357778048669573 ) ) ;
#16719 = EDGE_CURVE ( 'NONE', #10789, #2247, #15651, .T. ) ;
#16720 = ORIENTED_EDGE ( 'NONE', *, *, #8934, .F. ) ;
#16721 = CARTESIAN_POINT ( 'NONE',  ( 29.30958546476020743, -4.505622649006972402, 3.283357778048664244 ) ) ;
#16722 = EDGE_CURVE ( 'NONE', #13752, #14031, #15057, .T. ) ;
#16723 = AXIS2_PLACEMENT_3D ( 'NONE', #4557, #7471, #14558 ) ;
#16724 = CARTESIAN_POINT ( 'NONE',  ( 26.39823381822651882, -6.110324093391315436, 7.939653947423658487 ) ) ;
#16725 = SURFACE_SIDE_STYLE ('',( #11438 ) ) ;
#16726 = FACE_BOUND ( 'NONE', #4477, .T. ) ;
#16727 = ORIENTED_EDGE ( 'NONE', *, *, #12056, .F. ) ;
#16728 = CARTESIAN_POINT ( 'NONE',  ( 32.58190297908952004, -5.565186596593329149, -8.283357778048664244 ) ) ;
#16729 = VERTEX_POINT ( 'NONE', #1886 ) ;
#16730 = ORIENTED_EDGE ( 'NONE', *, *, #9109, .F. ) ;
#16731 = DIRECTION ( 'NONE',  ( -0.000000000000000000, -0.000000000000000000, -1.000000000000000000 ) ) ;
#16732 = CARTESIAN_POINT ( 'NONE',  ( 26.01127209431523113, -6.877383572197488526, -7.035051132944705188 ) ) ;
#16733 = VERTEX_POINT ( 'NONE', #11553 ) ;
#16734 = CARTESIAN_POINT ( 'NONE',  ( 39.16489837658902218, -5.353591089051433549, -2.283357778048670461 ) ) ;
#16735 = CARTESIAN_POINT ( 'NONE',  ( -4.000000000000000888, 1.563622288139197458, -0.2253451193528329122 ) ) ;
#16736 = DIRECTION ( 'NONE',  ( 5.551115123125782702E-17, -2.775557561562891351E-16, 0.9999999999999998890 ) ) ;
#16737 = DIRECTION ( 'NONE',  ( 0.000000000000000000, 0.000000000000000000, -1.000000000000000000 ) ) ;
#16738 = CARTESIAN_POINT ( 'NONE',  ( 29.49337484321020497, -2.602568060005117090, 6.861505862736165362 ) ) ;
#16739 = VECTOR ( 'NONE', #12596, 1000.000000000000000 ) ;
#16740 = CARTESIAN_POINT ( 'NONE',  ( 31.89397184978405519, -6.712334120981523711, 5.783357778048664244 ) ) ;
#16741 = DIRECTION ( 'NONE',  ( 0.000000000000000000, 0.000000000000000000, 1.000000000000000000 ) ) ;
#16742 = CARTESIAN_POINT ( 'NONE',  ( 31.87075164095941915, -4.197052703815608687, 7.939653947423662039 ) ) ;
#16743 = EDGE_LOOP ( 'NONE', ( #9614, #8874, #8455, #14008 ) ) ;
#16744 = CIRCLE ( 'NONE', #7202, 6.249999999999998224 ) ;
#16745 = VERTEX_POINT ( 'NONE', #4495 ) ;
#16746 = CARTESIAN_POINT ( 'NONE',  ( 29.62489513447700062, -6.348545659133139729, 4.705209693361160461 ) ) ;
#16747 = SURFACE_STYLE_FILL_AREA ( #11372 ) ;
#16748 = FACE_OUTER_BOUND ( 'NONE', #3037, .T. ) ;
#16749 = ORIENTED_EDGE ( 'NONE', *, *, #1038, .T. ) ;
#16750 = CARTESIAN_POINT ( 'NONE',  ( 26.19678349485696955, -4.880653813392439311, 7.939653947423662039 ) ) ;
#16751 = DIRECTION ( 'NONE',  ( -0.000000000000000000, -0.000000000000000000, 1.000000000000000000 ) ) ;
#16752 = AXIS2_PLACEMENT_3D ( 'NONE', #15410, #369, #12953 ) ;
#16753 = CARTESIAN_POINT ( 'NONE',  ( 26.31556265977298992, -7.384422263489805793, 5.783357778048663356 ) ) ;
#16754 = EDGE_CURVE ( 'NONE', #1701, #2990, #17120, .T. ) ;
#16755 = DIRECTION ( 'NONE',  ( 0.9928203230275510771, 0.1196152422706614621, -0.000000000000000000 ) ) ;
#16756 = CARTESIAN_POINT ( 'NONE',  ( 27.04606801335823718, -3.524390735323772006, -7.939653947423660263 ) ) ;
#16757 = DIRECTION ( 'NONE',  ( 1.000000000000000000, 0.000000000000000000, 0.000000000000000000 ) ) ;
#16758 = CARTESIAN_POINT ( 'NONE',  ( 30.69058026372202974, -5.793053633118939061, -8.283357778048662468 ) ) ;
#16759 = FACE_OUTER_BOUND ( 'NONE', #14917, .T. ) ;
#16760 = LINE ( 'NONE', #4510, #16791 ) ;
#16761 = PRESENTATION_STYLE_ASSIGNMENT (( #17138 ) ) ;
#16762 = CARTESIAN_POINT ( 'NONE',  ( 30.64918316926811315, -2.463315982128351678, -6.861505862736159145 ) ) ;
#16763 = ORIENTED_EDGE ( 'NONE', *, *, #4209, .F. ) ;
#16764 = CARTESIAN_POINT ( 'NONE',  ( 26.03655646321512052, -5.068638614726478586, -8.187879365734106685 ) ) ;
#16765 = CARTESIAN_POINT ( 'NONE',  ( 30.48043329534786849, -5.818372192732907067, -3.283357778048667797 ) ) ;
#16766 = VECTOR ( 'NONE', #5435, 1000.000000000000000 ) ;
#16767 = ORIENTED_EDGE ( 'NONE', *, *, #13327, .T. ) ;
#16768 = ORIENTED_EDGE ( 'NONE', *, *, #10796, .F. ) ;
#16769 = ORIENTED_EDGE ( 'NONE', *, *, #9212, .F. ) ;
#16770 = CARTESIAN_POINT ( 'NONE',  ( 30.25080928106424594, -3.138282701210941994, 7.939653947423662927 ) ) ;
#16771 = VERTEX_POINT ( 'NONE', #13016 ) ;
#16772 = VECTOR ( 'NONE', #9819, 999.9999999999998863 ) ;
#16773 = CARTESIAN_POINT ( 'NONE',  ( 28.45891156537951971, -2.090033060632186412, -5.783357778048670461 ) ) ;
#16774 = CARTESIAN_POINT ( 'NONE',  ( 26.01652455409633902, -4.902371455920928156, -5.783357778048663356 ) ) ;
#16775 = DIRECTION ( 'NONE',  ( 0.000000000000000000, 0.000000000000000000, 1.000000000000000000 ) ) ;
#16776 = EDGE_CURVE ( 'NONE', #16631, #4593, #1862, .T. ) ;
#16777 = DIRECTION ( 'NONE',  ( 0.000000000000000000, 0.000000000000000000, -1.000000000000000000 ) ) ;
#16778 = CARTESIAN_POINT ( 'NONE',  ( 29.39282811755836633, -5.749534618892433002, -3.627061608673667781 ) ) ;
#16779 = CARTESIAN_POINT ( 'NONE',  ( 31.15208055228630357, -2.102918000029084578, -4.533357778048659803 ) ) ;
#16780 = ADVANCED_FACE ( 'NONE', ( #4100 ), #12164, .T. ) ;
#16781 = DIRECTION ( 'NONE',  ( 0.9928203230275510771, 0.1196152422706609902, 4.006172263299092517E-17 ) ) ;
#16782 = ORIENTED_EDGE ( 'NONE', *, *, #13199, .T. ) ;
#16783 = CONICAL_SURFACE ( 'NONE', #11239, 2.540000000000001368, 0.7853981633974502774 ) ;
#16784 = DIRECTION ( 'NONE',  ( 0.000000000000000000, 0.000000000000000000, 1.000000000000000000 ) ) ;
#16785 = CARTESIAN_POINT ( 'NONE',  ( 30.01512236704901682, -6.601339762873093875, -7.033357778048666908 ) ) ;
#16786 = ORIENTED_EDGE ( 'NONE', *, *, #16660, .T. ) ;
#16787 = CARTESIAN_POINT ( 'NONE',  ( 28.73594040535616756, -2.066853418799292630, -5.783357778048658027 ) ) ;
#16788 = DIRECTION ( 'NONE',  ( -1.000000000000000000, 0.000000000000000000, 0.000000000000000000 ) ) ;
#16789 = LINE ( 'NONE', #4452, #8633 ) ;
#16790 = ORIENTED_EDGE ( 'NONE', *, *, #16754, .F. ) ;
#16791 = VECTOR ( 'NONE', #11473, 1000.000000000000000 ) ;
#16792 = VECTOR ( 'NONE', #3108, 1000.000000000000227 ) ;
#16793 = CARTESIAN_POINT ( 'NONE',  ( -1.500000000000000666, -5.809475019311125976, -1.901951201008075243 ) ) ;
#16794 = CARTESIAN_POINT ( 'NONE',  ( 30.80688261270428541, -4.325227911964988792, 8.283357778048662468 ) ) ;
#16795 = CARTESIAN_POINT ( 'NONE',  ( 29.38830135902312080, -2.615227339812091767, -6.861505862736159145 ) ) ;
#16796 = AXIS2_PLACEMENT_3D ( 'NONE', #2728, #15228, #16506 ) ;
#16797 = ORIENTED_EDGE ( 'NONE', *, *, #6228, .T. ) ;
#16798 = ORIENTED_EDGE ( 'NONE', *, *, #14304, .F. ) ;
#16799 = FACE_OUTER_BOUND ( 'NONE', #10740, .T. ) ;
#16800 = CARTESIAN_POINT ( 'NONE',  ( 29.71979337562451207, -1.938121702948446323, -5.783357778048664244 ) ) ;
#16801 = EDGE_CURVE ( 'NONE', #8474, #7363, #1210, .T. ) ;
#16802 = EDGE_LOOP ( 'NONE', ( #5668, #17158, #8462, #4494, #1891, #12367, #546, #5716, #8598 ) ) ;
#16803 = CARTESIAN_POINT ( 'NONE',  ( -24.42951923951777005, -10.13045284482685382, -14.60898600760630472 ) ) ;
#16804 = ORIENTED_EDGE ( 'NONE', *, *, #17955, .F. ) ;
#16805 = VECTOR ( 'NONE', #6295, 1000.000000000000227 ) ;
#16806 = EDGE_CURVE ( 'NONE', #16322, #6149, #3555, .T. ) ;
#16807 = CARTESIAN_POINT ( 'NONE',  ( 27.28266178881210280, -7.257709054644825741, -5.783357778048669573 ) ) ;
#16808 = ORIENTED_EDGE ( 'NONE', *, *, #9739, .F. ) ;
#16809 = ORIENTED_EDGE ( 'NONE', *, *, #15161, .T. ) ;
#16810 = VECTOR ( 'NONE', #16384, 1000.000000000000227 ) ;
#16811 = CARTESIAN_POINT ( 'NONE',  ( 31.91006497951310550, -2.311404624444611589, -6.861505862736159145 ) ) ;
#16812 = EDGE_CURVE ( 'NONE', #14428, #13470, #13150, .T. ) ;
#16813 = DIRECTION ( 'NONE',  ( 0.000000000000000000, 0.000000000000000000, 1.000000000000000000 ) ) ;
#16814 = CARTESIAN_POINT ( 'NONE',  ( 4.197310878070204865, 0.8178547585014688259, -3.202500312981938269 ) ) ;
#16815 = CARTESIAN_POINT ( 'NONE',  ( 32.47301885516785092, -2.670677813450649474, -3.283357778048662023 ) ) ;
#16816 = CARTESIAN_POINT ( 'NONE',  ( 31.63243098167119172, -2.771952051906466430, -8.283357778048660691 ) ) ;
#16817 = CIRCLE ( 'NONE', #9280, 5.500000000000000000 ) ;
#16818 = CARTESIAN_POINT ( 'NONE',  ( 33.19286683830256379, -2.783822866615540903, 3.627061608673666893 ) ) ;
#16819 = CARTESIAN_POINT ( 'NONE',  ( 27.25621498173240198, -3.499072175709823984, 7.939653947423664704 ) ) ;
#16820 = CARTESIAN_POINT ( 'NONE',  ( -17.40358024347774091, -19.00834140588416332, 15.93963985190277910 ) ) ;
#16821 = FACE_OUTER_BOUND ( 'NONE', #9672, .T. ) ;
#16822 = VERTEX_POINT ( 'NONE', #9609 ) ;
#16823 = CARTESIAN_POINT ( 'NONE',  ( 26.24611652476386681, -6.808011323847543927, -7.414850139186299316 ) ) ;
#16824 = ORIENTED_EDGE ( 'NONE', *, *, #15798, .F. ) ;
#16825 = CARTESIAN_POINT ( 'NONE',  ( -35.74085044863416272, -28.97437970944926988, -11.27079897466147607 ) ) ;
#16826 = EDGE_CURVE ( 'NONE', #3360, #5903, #10871, .T. ) ;
#16827 = ORIENTED_EDGE ( 'NONE', *, *, #2848, .T. ) ;
#16828 = CARTESIAN_POINT ( 'NONE',  ( 30.40162818048570514, -5.827866652795590241, -3.283357778048667797 ) ) ;
#16829 = VECTOR ( 'NONE', #15145, 1000.000000000000227 ) ;
#16830 = AXIS2_PLACEMENT_3D ( 'NONE', #8911, #7463, #2030 ) ;
#16831 = CARTESIAN_POINT ( 'NONE',  ( 33.48996557372703364, -1.821249024531260696, -7.033357778048658027 ) ) ;
#16832 = CARTESIAN_POINT ( 'NONE',  ( 31.04700706809921940, -2.115577279836057922, -7.033357778048658027 ) ) ;
#16833 = DIRECTION ( 'NONE',  ( -0.1196152422706610735, 0.9928203230275511881, 0.000000000000000000 ) ) ;
#16834 = SHAPE_DEFINITION_REPRESENTATION ( #1445, #12009 ) ;
#16835 = CARTESIAN_POINT ( 'NONE',  ( 0.000000000000000000, 0.000000000000000000, 1.159999999999999476 ) ) ;
#16836 = EDGE_CURVE ( 'NONE', #6589, #11736, #16441, .T. ) ;
#16837 = CARTESIAN_POINT ( 'NONE',  ( 32.87199790123699472, -1.558343308739095656, 5.783357778048663356 ) ) ;
#16838 = VECTOR ( 'NONE', #8886, 1000.000000000000000 ) ;
#16839 = CARTESIAN_POINT ( 'NONE',  ( 28.01872616749444944, -6.841866079205687790, -4.533357778048668685 ) ) ;
#16840 = CARTESIAN_POINT ( 'NONE',  ( 5.200000000000002842, 0.000000000000000000, 0.000000000000000000 ) ) ;
#16841 = CARTESIAN_POINT ( 'NONE',  ( 29.56783163384821833, -3.220568019956291383, 3.627061608673666893 ) ) ;
#16842 = ORIENTED_EDGE ( 'NONE', *, *, #15189, .F. ) ;
#16843 = VECTOR ( 'NONE', #16516, 1000.000000000000000 ) ;
#16844 = ORIENTED_EDGE ( 'NONE', *, *, #8272, .T. ) ;
#16845 = CARTESIAN_POINT ( 'NONE',  ( 27.51889869220010354, -3.467423976192371082, 3.627061608673666893 ) ) ;
#16846 = DIRECTION ( 'NONE',  ( -0.1196152422706610735, 0.9928203230275511881, 0.000000000000000000 ) ) ;
#16847 = DIRECTION ( 'NONE',  ( 0.9928203230275512992, 0.1196152422706607682, -0.000000000000000000 ) ) ;
#16848 = EDGE_LOOP ( 'NONE', ( #8597, #9525 ) ) ;
#16849 = CARTESIAN_POINT ( 'NONE',  ( 26.52522735095806894, -6.721994413439005278, 6.861505862736157368 ) ) ;
#16850 = ORIENTED_EDGE ( 'NONE', *, *, #2146, .F. ) ;
#16851 = CARTESIAN_POINT ( 'NONE',  ( 34.91600907648203389, -11.88801210197604341, 0.000000000000000000 ) ) ;
#16852 = DIRECTION ( 'NONE',  ( 1.000000000000000000, 0.000000000000000000, 0.000000000000000000 ) ) ;
#16853 = EDGE_CURVE ( 'NONE', #6903, #9826, #1875, .T. ) ;
#16854 = CARTESIAN_POINT ( 'NONE',  ( 29.42285898892238549, -7.010054420087358018, 6.453230759126468818 ) ) ;
#16855 = CARTESIAN_POINT ( 'NONE',  ( -1.500000000000000000, 11.00000000000000000, -3.000000000000000000 ) ) ;
#16856 = LINE ( 'NONE', #8404, #7630 ) ;
#16857 = EDGE_LOOP ( 'NONE', ( #859, #15835, #8579, #6256, #9222, #15472 ) ) ;
#16858 = CARTESIAN_POINT ( 'NONE',  ( 29.35841309260160159, -6.680460261459264970, -4.533357778048668685 ) ) ;
#16859 = CARTESIAN_POINT ( 'NONE',  ( 33.18226487515251932, -2.585227674546096477, -3.283357778048662023 ) ) ;
#16860 = VECTOR ( 'NONE', #14210, 999.9999999999998863 ) ;
#16861 = DIRECTION ( 'NONE',  ( 1.224646799147353207E-16, 1.000000000000000000, 0.000000000000000000 ) ) ;
#16862 = CARTESIAN_POINT ( 'NONE',  ( 32.77709966008947617, -5.968767264923789284, -6.861505862736166250 ) ) ;
#16863 = VERTEX_POINT ( 'NONE', #1382 ) ;
#16864 = AXIS2_PLACEMENT_3D ( 'NONE', #10865, #1461, #4356 ) ;
#16865 = CARTESIAN_POINT ( 'NONE',  ( 25.76466184735054910, -2.811881907026620553, -6.248149982130924762 ) ) ;
#16866 = CARTESIAN_POINT ( 'NONE',  ( 27.45273115869273539, -7.247415916675651992, -5.113484796970856117 ) ) ;
#16867 = AXIS2_PLACEMENT_3D ( 'NONE', #15056, #10948, #5607 ) ;
#16868 = EDGE_CURVE ( 'NONE', #9939, #7023, #5606, .T. ) ;
#16869 = ORIENTED_EDGE ( 'NONE', *, *, #17716, .T. ) ;
#16870 = ORIENTED_EDGE ( 'NONE', *, *, #6385, .F. ) ;
#16871 = ORIENTED_EDGE ( 'NONE', *, *, #1019, .F. ) ;
#16872 = VERTEX_POINT ( 'NONE', #12264 ) ;
#16873 = CARTESIAN_POINT ( 'NONE',  ( 26.97161122272022382, -2.906390775372597712, 6.861505862736165362 ) ) ;
#16874 = AXIS2_PLACEMENT_3D ( 'NONE', #3967, #13668, #8306 ) ;
#16875 = CARTESIAN_POINT ( 'NONE',  ( 25.29083129957448151, -4.989803161779970964, -5.783357778048664244 ) ) ;
#16876 = DIRECTION ( 'NONE',  ( -0.000000000000000000, -0.000000000000000000, -1.000000000000000000 ) ) ;
#16877 = CARTESIAN_POINT ( 'NONE',  ( -23.00000000000000000, -16.21813761408365195, 13.00000000000000178 ) ) ;
#16878 = DIRECTION ( 'NONE',  ( 0.000000000000000000, 0.000000000000000000, 1.000000000000000000 ) ) ;
#16879 = CARTESIAN_POINT ( 'NONE',  ( 31.41531425212677675, -1.744041783721344219, -5.783357778048658027 ) ) ;
#16880 = DIRECTION ( 'NONE',  ( -1.000000000000000000, -0.000000000000000000, -0.000000000000000000 ) ) ;
#16881 = PLANE ( 'NONE',  #4361 ) ;
#16882 = CONICAL_SURFACE ( 'NONE', #2117, 3.500000000000004885, 0.1745329251994333364 ) ;
#16883 = AXIS2_PLACEMENT_3D ( 'NONE', #9492, #13847, #10664 ) ;
#16884 = CARTESIAN_POINT ( 'NONE',  ( -23.02601376483258022, 3.965314980223224151, -6.000000000000000000 ) ) ;
#16885 = DIRECTION ( 'NONE',  ( 1.000000000000000000, -1.421085471520200372E-14, 0.000000000000000000 ) ) ;
#16886 = ORIENTED_EDGE ( 'NONE', *, *, #12382, .F. ) ;
#16887 = CARTESIAN_POINT ( 'NONE',  ( 31.51621784984448738, -6.120678622607529817, -6.861505862736166250 ) ) ;
#16888 = CARTESIAN_POINT ( 'NONE',  ( -20.00000000000000000, 7.999999999999996447, 15.51150668642334374 ) ) ;
#16889 = CARTESIAN_POINT ( 'NONE',  ( 25.11802603177690330, -19.03270077640483038, 0.5379818257722508434 ) ) ;
#16890 = CARTESIAN_POINT ( 'NONE',  ( 25.74999999999999289, -16.21813761408365195, -13.00000000000000178 ) ) ;
#16891 = ORIENTED_EDGE ( 'NONE', *, *, #8915, .T. ) ;
#16892 = CARTESIAN_POINT ( 'NONE',  ( 26.85044460880409645, -7.319979551716484067, 5.783357778048657138 ) ) ;
#16893 = AXIS2_PLACEMENT_3D ( 'NONE', #6576, #6660, #12191 ) ;
#16894 = EDGE_CURVE ( 'NONE', #17327, #16872, #8266, .T. ) ;
#16895 = CARTESIAN_POINT ( 'NONE',  ( 29.11066736118121057, -3.075774767273946608, 3.283357778048666464 ) ) ;
#16896 = CARTESIAN_POINT ( 'NONE',  ( 26.47269060886452507, -6.728324053342490174, -6.861505862736166250 ) ) ;
#16897 = VERTEX_POINT ( 'NONE', #5532 ) ;
#16898 = ORIENTED_EDGE ( 'NONE', *, *, #17864, .T. ) ;
#16899 = CARTESIAN_POINT ( 'NONE',  ( 0.000000000000000000, 0.000000000000000000, -4.000000000000000000 ) ) ;
#16900 = CARTESIAN_POINT ( 'NONE',  ( 26.92924972366625980, -7.310485091653801781, -5.783357778048657138 ) ) ;
#16901 = VERTEX_POINT ( 'NONE', #11057 ) ;
#16902 = DIRECTION ( 'NONE',  ( 0.1195020427801297691, 0.9918807541847894926, -0.04349518650597275493 ) ) ;
#16903 = ORIENTED_EDGE ( 'NONE', *, *, #15038, .T. ) ;
#16904 = VECTOR ( 'NONE', #17661, 1000.000000000000000 ) ;
#16905 = CARTESIAN_POINT ( 'NONE',  ( 27.25621498173240198, -3.499072175709823984, -3.627061608673662008 ) ) ;
#16906 = CIRCLE ( 'NONE', #9080, 6.000000000000000888 ) ;
#16908 = EDGE_LOOP ( 'NONE', ( #9356, #7923, #8572, #2826 ) ) ;
#16907 =( BOUNDED_CURVE ( )  B_SPLINE_CURVE ( 2, ( #11246, #1499, #14007, #11156, #1316, #16728, #2677, #8206, #13733 ),
 .UNSPECIFIED., .F., .T. ) 
 B_SPLINE_CURVE_WITH_KNOTS ( ( 3, 2, 2, 2, 3 ),
 ( 0.09615384615384617306, 0.1025641025641025605, 0.1153846153846153910, 0.1282051282051281937, 0.1346153846153846367 ),
 .UNSPECIFIED. ) 
 CURVE ( )  GEOMETRIC_REPRESENTATION_ITEM ( )  RATIONAL_B_SPLINE_CURVE ( ( 0.9330127018922194093, 0.9330127018922196314, 1.000000000000000000, 0.8660254037844387076, 1.000000000000000000, 0.8660254037844387076, 1.000000000000000000, 0.9330127018922190762, 0.9330127018922194093 ) ) 
 REPRESENTATION_ITEM ( '' )  );
#16909 = CARTESIAN_POINT ( 'NONE',  ( 31.30154412293507349, -3.011689903141150815, -7.939653947423660263 ) ) ;
#16910 = DIRECTION ( 'NONE',  ( -0.1196152422706611984, 0.9928203230275510771, 0.000000000000000000 ) ) ;
#16911 = DIRECTION ( 'NONE',  ( -0.000000000000000000, 1.000000000000000000, 0.000000000000000000 ) ) ;
#16912 = CARTESIAN_POINT ( 'NONE',  ( 27.50903986916043920, -7.240631829073577386, 5.113484796970857005 ) ) ;
#16913 = CARTESIAN_POINT ( 'NONE',  ( 31.70371634254663817, -2.036456781249897485, -4.533357778048659803 ) ) ;
#16914 = EDGE_CURVE ( 'NONE', #2781, #3845, #937, .T. ) ;
#16915 = LINE ( 'NONE', #12812, #4546 ) ;
#16916 = ORIENTED_EDGE ( 'NONE', *, *, #11922, .T. ) ;
#16917 = CARTESIAN_POINT ( 'NONE',  ( 32.01513846370018967, -2.298745344637636912, 6.861505862736165362 ) ) ;
#16918 = CARTESIAN_POINT ( 'NONE',  ( 27.86926259684567597, -5.933094176093606897, 3.627061608673662896 ) ) ;
#16919 = CARTESIAN_POINT ( 'NONE',  ( -29.25000000000000000, -16.63595338719256844, 13.37255996287877124 ) ) ;
#16920 = FACE_OUTER_BOUND ( 'NONE', #5137, .T. ) ;
#16921 = ORIENTED_EDGE ( 'NONE', *, *, #6696, .T. ) ;
#16922 = ORIENTED_EDGE ( 'NONE', *, *, #6655, .T. ) ;
#16923 = DIRECTION ( 'NONE',  ( 0.000000000000000000, 0.000000000000000000, 1.000000000000000000 ) ) ;
#16924 = EDGE_LOOP ( 'NONE', ( #15198, #1771, #8815, #13515 ) ) ;
#16925 = CARTESIAN_POINT ( 'NONE',  ( 26.01652455409633902, -4.902371455920926380, -5.783357778048663356 ) ) ;
#16926 = CARTESIAN_POINT ( 'NONE',  ( 33.45617745041539592, -1.098413033681664430, -5.783357778048658027 ) ) ;
#16927 = FACE_OUTER_BOUND ( 'NONE', #17032, .T. ) ;
#16928 = DIRECTION ( 'NONE',  ( -0.000000000000000000, -0.000000000000000000, -1.000000000000000000 ) ) ;
#16929 = SHAPE_DEFINITION_REPRESENTATION ( #11844, #16332 ) ;
#16930 = FACE_OUTER_BOUND ( 'NONE', #12926, .T. ) ;
#16931 = CARTESIAN_POINT ( 'NONE',  ( 29.56783163384821833, -3.220568019956291383, -7.939653947423660263 ) ) ;
#16932 = CARTESIAN_POINT ( 'NONE',  ( 32.18597209352066812, -4.159074864394664672, -7.939653947423662039 ) ) ;
#16933 = DIRECTION ( 'NONE',  ( 5.026720092345836698E-22, -4.581671729415424240E-22, 1.000000000000000000 ) ) ;
#16934 = CYLINDRICAL_SURFACE ( 'NONE', #6319, 2.500000000000001776 ) ;
#16935 = CARTESIAN_POINT ( 'NONE',  ( 30.60986983071443390, -4.348964061499348333, 7.939653947423662039 ) ) ;
#16936 = EDGE_CURVE ( 'NONE', #14370, #4798, #17405, .T. ) ;
#16937 = ORIENTED_EDGE ( 'NONE', *, *, #3228, .T. ) ;
#16938 = ORIENTED_EDGE ( 'NONE', *, *, #6802, .T. ) ;
#16939 = CARTESIAN_POINT ( 'NONE',  ( 27.09860475545177039, -3.518061095420291995, 7.939653947423664704 ) ) ;
#16940 = CARTESIAN_POINT ( 'NONE',  ( 31.94462260941237020, -6.706231704719880504, -5.113484796970860558 ) ) ;
#16941 = DIRECTION ( 'NONE',  ( -1.000000000000000000, 0.000000000000000000, 0.000000000000000000 ) ) ;
#16942 = EDGE_CURVE ( 'NONE', #8853, #15406, #9122, .T. ) ;
#16943 = VERTEX_POINT ( 'NONE', #6904 ) ;
#16944 = CARTESIAN_POINT ( 'NONE',  ( 26.51200394741821498, -4.842675973971495296, 3.627061608673664228 ) ) ;
#16945 = DIRECTION ( 'NONE',  ( -0.000000000000000000, -0.000000000000000000, 1.000000000000000000 ) ) ;
#16946 = ORIENTED_EDGE ( 'NONE', *, *, #1611, .F. ) ;
#16947 = CARTESIAN_POINT ( 'NONE',  ( 36.27615609941022257, -23.17738945083361557, 0.000000000000000000 ) ) ;
#16948 = DIRECTION ( 'NONE',  ( -1.224646799147353207E-16, 1.000000000000000000, 0.000000000000000000 ) ) ;
#16949 = DIRECTION ( 'NONE',  ( 0.9928203230275510771, 0.1196152422706609902, 4.006172263299092517E-17 ) ) ;
#16950 = CARTESIAN_POINT ( 'NONE',  ( 26.34507017448785504, -7.770415366711231009, -5.783357778048669573 ) ) ;
#16951 = ORIENTED_EDGE ( 'NONE', *, *, #9983, .F. ) ;
#16952 = CARTESIAN_POINT ( 'NONE',  ( 32.95080301609915097, -1.548848848676412260, -5.783357778048662468 ) ) ;
#16953 = DIRECTION ( 'NONE',  ( -1.000000000000000000, -0.000000000000000000, -0.000000000000000000 ) ) ;
#16954 = SURFACE_SIDE_STYLE ('',( #8589 ) ) ;
#16955 = CARTESIAN_POINT ( 'NONE',  ( 32.12473870642251939, -5.420393343910986594, -7.939653947423664704 ) ) ;
#16956 = CARTESIAN_POINT ( 'NONE',  ( 26.51200394741821498, -4.842675973971495296, -7.939653947423662039 ) ) ;
#16957 = CARTESIAN_POINT ( 'NONE',  ( 26.59574320524588842, -2.314508053356755024, -5.113484796970857893 ) ) ;
#16958 = EDGE_CURVE ( 'NONE', #4593, #17725, #6722, .T. ) ;
#16959 = ORIENTED_EDGE ( 'NONE', *, *, #3292, .F. ) ;
#16960 = ORIENTED_EDGE ( 'NONE', *, *, #8484, .F. ) ;
#16961 = CARTESIAN_POINT ( 'NONE',  ( 29.38830135902312080, -2.615227339812091767, 4.705209693361167567 ) ) ;
#16962 = EDGE_CURVE ( 'NONE', #2920, #10340, #7733, .T. ) ;
#16963 = CARTESIAN_POINT ( 'NONE',  ( -20.00000000000000355, 7.999999999999996447, 0.000000000000000000 ) ) ;
#16964 = DIRECTION ( 'NONE',  ( -0.000000000000000000, -1.000000000000000000, -0.000000000000000000 ) ) ;
#16965 = DIRECTION ( 'NONE',  ( -4.179998415399335043E-17, -3.469446951953615175E-16, 1.000000000000000000 ) ) ;
#16966 = DIRECTION ( 'NONE',  ( 0.1113444980252557837, -0.9937818688019538493, 0.000000000000000000 ) ) ;
#16967 = CARTESIAN_POINT ( 'NONE',  ( 31.56875459193803124, -6.114348982704044921, -4.705209693361169343 ) ) ;
#16968 = CARTESIAN_POINT ( 'NONE',  ( 31.68992120585416217, -1.700760206360153015, -5.783357778048664244 ) ) ;
#16969 = CARTESIAN_POINT ( 'NONE',  ( -3.999999999999998224, 0.000000000000000000, 0.000000000000000000 ) ) ;
#16970 = CARTESIAN_POINT ( 'NONE',  ( 34.91600907648203389, -11.88801210197604341, -12.00000000000000000 ) ) ;
#16971 = EDGE_CURVE ( 'NONE', #3112, #6328, #13978, .T. ) ;
#16972 = DIRECTION ( 'NONE',  ( -0.000000000000000000, 0.000000000000000000, -1.000000000000000000 ) ) ;
#16973 = ORIENTED_EDGE ( 'NONE', *, *, #6097, .T. ) ;
#16974 = CARTESIAN_POINT ( 'NONE',  ( 30.76748005699505129, -4.329975141788874993, -7.939653947423662039 ) ) ;
#16975 = CARTESIAN_POINT ( 'NONE',  ( 0.000000000000000000, 0.000000000000000000, 0.000000000000000000 ) ) ;
#16976 = CARTESIAN_POINT ( 'NONE',  ( 34.91600907648203389, -11.88801210197604341, 12.00000000000000000 ) ) ;
#16977 = DIRECTION ( 'NONE',  ( -0.000000000000000000, -0.000000000000000000, -1.000000000000000000 ) ) ;
#16978 = CARTESIAN_POINT ( 'NONE',  ( 26.16860980394290337, -3.430234601869349920, 8.283357778048666020 ) ) ;
#16979 = ADVANCED_FACE ( 'NONE', ( #17077, #8725 ), #4630, .T. ) ;
#16980 = CARTESIAN_POINT ( 'NONE',  ( 28.78802868011566929, -7.476087111406434893, 5.783357778048657138 ) ) ;
#16981 = CYLINDRICAL_SURFACE ( 'NONE', #4260, 2.500000000000001776 ) ;
#16982 = ORIENTED_EDGE ( 'NONE', *, *, #17544, .T. ) ;
#16983 = ORIENTED_EDGE ( 'NONE', *, *, #6062, .F. ) ;
#16984 = CARTESIAN_POINT ( 'NONE',  ( 33.60446413004628141, -3.988174587000466342, -3.627061608673664672 ) ) ;
#16985 = EDGE_LOOP ( 'NONE', ( #4870, #10571, #405, #7384 ) ) ;
#16986 = ORIENTED_EDGE ( 'NONE', *, *, #4996, .T. ) ;
#16987 = CARTESIAN_POINT ( 'NONE',  ( 0.000000000000000000, 2.357898499370432166, -2.385244779468109755E-15 ) ) ;
#16988 = EDGE_LOOP ( 'NONE', ( #8045, #5750, #10246, #11734 ) ) ;
#16989 =( BOUNDED_CURVE ( )  B_SPLINE_CURVE ( 2, ( #887, #8955, #2436, #11937, #711, #11671, #14499, #10650, #12024 ),
 .UNSPECIFIED., .F., .T. ) 
 B_SPLINE_CURVE_WITH_KNOTS ( ( 3, 2, 2, 2, 3 ),
 ( 0.1346153846153846367, 0.1410256410256410242, 0.1538461538461538547, 0.1666666666666666574, 0.1730769230769231004 ),
 .UNSPECIFIED. ) 
 CURVE ( )  GEOMETRIC_REPRESENTATION_ITEM ( )  RATIONAL_B_SPLINE_CURVE ( ( 0.9330127018922194093, 0.9330127018922196314, 1.000000000000000000, 0.8660254037844387076, 1.000000000000000000, 0.8660254037844387076, 1.000000000000000000, 0.9330127018922190762, 0.9330127018922194093 ) ) 
 REPRESENTATION_ITEM ( '' )  );
#16990 = CARTESIAN_POINT ( 'NONE',  ( 26.65222088368961195, -7.333664733486695120, -5.783357778048669573 ) ) ;
#16991 = ADVANCED_FACE ( 'NONE', ( #1567 ), #15705, .T. ) ;
#16992 = CARTESIAN_POINT ( 'NONE',  ( 31.51621784984448738, -6.120678622607529817, -6.861505862736166250 ) ) ;
#16993 = VERTEX_POINT ( 'NONE', #11506 ) ;
#16994 = DIRECTION ( 'NONE',  ( 0.000000000000000000, 0.000000000000000000, 1.000000000000000000 ) ) ;
#16995 = CARTESIAN_POINT ( 'NONE',  ( 32.89331279191618762, -2.620040694222726785, -8.283357778048660691 ) ) ;
#16996 = CARTESIAN_POINT ( 'NONE',  ( 33.95908713831674675, -3.945449517755637903, -5.783357778048663356 ) ) ;
#16997 = VERTEX_POINT ( 'NONE', #14349 ) ;
#16998 = CARTESIAN_POINT ( 'NONE',  ( 33.01342578063301403, -4.059383036018435753, -8.283357778048662468 ) ) ;
#16999 = EDGE_CURVE ( 'NONE', #11418, #7303, #17520, .T. ) ;
#17000 = DIRECTION ( 'NONE',  ( -1.000000000000000000, 0.000000000000000000, 0.000000000000000000 ) ) ;
#17001 = EDGE_CURVE ( 'NONE', #17122, #5005, #15432, .T. ) ;
#17002 = CARTESIAN_POINT ( 'NONE',  ( 31.71314141467879111, -4.216041623526076698, 7.939653947423662039 ) ) ;
#17003 = FACE_OUTER_BOUND ( 'NONE', #17530, .T. ) ;
#17004 = CARTESIAN_POINT ( 'NONE',  ( -23.43613571611706803, -22.46619466838626877, 14.83130101496670861 ) ) ;
#17005 = DIRECTION ( 'NONE',  ( -0.000000000000000000, -0.000000000000000000, -1.000000000000000000 ) ) ;
#17006 = ORIENTED_EDGE ( 'NONE', *, *, #12395, .T. ) ;
#17007 = DIRECTION ( 'NONE',  ( 1.000000000000000000, 4.440892098500626162E-15, 0.000000000000000000 ) ) ;
#17008 = VERTEX_POINT ( 'NONE', #12794 ) ;
#17009 = DIRECTION ( 'NONE',  ( 0.9928203230275512992, 0.1196152422706610180, 4.006172263299093133E-17 ) ) ;
#17010 = DIRECTION ( 'NONE',  ( 0.9899494936611662466, -0.1414213562373111965, -0.000000000000000000 ) ) ;
#17011 = EDGE_CURVE ( 'NONE', #5885, #9480, #9560, .T. ) ;
#17012 = ORIENTED_EDGE ( 'NONE', *, *, #10188, .T. ) ;
#17013 = CARTESIAN_POINT ( 'NONE',  ( 0.000000000000000000, 0.000000000000000000, -3.000000000000000000 ) ) ;
#17014 = ADVANCED_FACE ( 'NONE', ( #3285 ), #8625, .F. ) ;
#17015 = CARTESIAN_POINT ( 'NONE',  ( 27.88665588685489993, -3.423116496867954162, -3.627061608673662008 ) ) ;
#17016 = CARTESIAN_POINT ( 'NONE',  ( 32.90454166015506132, -1.164874252460851300, -5.783357778048658027 ) ) ;
#17017 = DIRECTION ( 'NONE',  ( 0.000000000000000000, 0.000000000000000000, -1.000000000000000000 ) ) ;
#17018 = PRODUCT_CONTEXT ( 'NONE', #17356, 'mechanical' ) ;
#17019 = DIRECTION ( 'NONE',  ( 1.000000000000000000, 0.000000000000000000, 0.000000000000000000 ) ) ;
#17020 = CARTESIAN_POINT ( 'NONE',  ( 28.26310972651430120, -2.123820177930694442, -5.783357778048658027 ) ) ;
#17021 = CARTESIAN_POINT ( 'NONE',  ( 33.43363050022580296, -2.127845067243429256, -4.705209693361160461 ) ) ;
#17022 = CARTESIAN_POINT ( 'NONE',  ( 41.90164972253718645, -2.988527579590353422, -5.783357778048662468 ) ) ;
#17023 = CARTESIAN_POINT ( 'NONE',  ( 33.69269431359690969, -6.158264969628857166, 7.033357778048657138 ) ) ;
#17024 = CARTESIAN_POINT ( 'NONE',  ( 29.17398450417959310, -7.029842018119214941, 5.783357778048657138 ) ) ;
#17025 = AXIS2_PLACEMENT_3D ( 'NONE', #5022, #5281, #16373 ) ;
#17026 = ORIENTED_EDGE ( 'NONE', *, *, #17, .F. ) ;
#17027 = CARTESIAN_POINT ( 'NONE',  ( 26.35439372113758694, -4.861664893681965083, -7.939653947423662039 ) ) ;
#17028 = ORIENTED_EDGE ( 'NONE', *, *, #17446, .F. ) ;
#17029 = CARTESIAN_POINT ( 'NONE',  ( 31.43723430067123914, -2.368371383576012956, 4.705209693361168455 ) ) ;
#17030 = DIRECTION ( 'NONE',  ( -1.000000000000000000, 0.000000000000000000, 0.000000000000000000 ) ) ;
#17031 = FACE_OUTER_BOUND ( 'NONE', #1128, .T. ) ;
#17032 = EDGE_LOOP ( 'NONE', ( #2679, #9852, #14338, #2241 ) ) ;
#17033 = CARTESIAN_POINT ( 'NONE',  ( 27.29814976067589072, -3.294147343736874234, 3.283357778048666464 ) ) ;
#17034 = CARTESIAN_POINT ( 'NONE',  ( -5.500000000000000000, -20.49999999999999645, -6.000000000000000000 ) ) ;
#17035 = CARTESIAN_POINT ( 'NONE',  ( 25.93714794488954212, -2.393855775999666591, -5.783357778048658027 ) ) ;
#17037 = EDGE_CURVE ( 'NONE', #5445, #2513, #5803, .T. ) ;
#17036 = CARTESIAN_POINT ( 'NONE',  ( 27.73348320195396965, -4.695511846111656062, -3.283357778048664688 ) ) ;
#17038 = CIRCLE ( 'NONE', #4282, 14.00000000000000178 ) ;
#17039 = CARTESIAN_POINT ( 'NONE',  ( 29.03578327489625011, -17.85349083735938081, 13.43326801114178615 ) ) ;
#17040 = DIRECTION ( 'NONE',  ( 0.000000000000000000, 0.000000000000000000, -1.000000000000000000 ) ) ;
#17041 = SHAPE_REPRESENTATION_RELATIONSHIP ( 'NONE' , 'NONE' ,  #2081, #14616 ) ;
#17042 = CARTESIAN_POINT ( 'NONE',  ( 31.91459173804834748, -5.445711903524953712, -3.627061608673667781 ) ) ;
#17043 = ORIENTED_EDGE ( 'NONE', *, *, #3192, .F. ) ;
#17044 = ADVANCED_FACE ( 'NONE', ( #11223 ), #1934, .T. ) ;
#17045 = CARTESIAN_POINT ( 'NONE',  ( -45.00000000000000711, 0.000000000000000000, 5.537981825772250843 ) ) ;
#17046 = CARTESIAN_POINT ( 'NONE',  ( 31.08079519141086777, -2.838413270685653078, 3.283357778048666464 ) ) ;
#17047 = ORIENTED_EDGE ( 'NONE', *, *, #17001, .T. ) ;
#17048 = VERTEX_POINT ( 'NONE', #11135 ) ;
#17049 = ORIENTED_EDGE ( 'NONE', *, *, #14455, .T. ) ;
#17050 = AXIS2_PLACEMENT_3D ( 'NONE', #12071, #16182, #11898 ) ;
#17051 = ORIENTED_EDGE ( 'NONE', *, *, #6111, .F. ) ;
#17052 = CARTESIAN_POINT ( 'NONE',  ( 29.39282811755836988, -5.749534618892433002, 7.939653947423658487 ) ) ;
#17053 = AXIS2_PLACEMENT_3D ( 'NONE', #1606, #14105, #10006 ) ;
#17054 = CARTESIAN_POINT ( 'NONE',  ( 31.89397184978405519, -6.712334120981523711, 5.783357778048664244 ) ) ;
#17055 = CYLINDRICAL_SURFACE ( 'NONE', #16180, 2.499999999999999112 ) ;
#17056 = CYLINDRICAL_SURFACE ( 'NONE', #5772, 6.249999999999998224 ) ;
#17057 = CARTESIAN_POINT ( 'NONE',  ( -19.22707546753401786, -21.21757778339487288, -15.64731278403363035 ) ) ;
#17058 = CARTESIAN_POINT ( 'NONE',  ( 31.03886041246737548, -3.043338102658604161, -3.627061608673662008 ) ) ;
#17059 = CARTESIAN_POINT ( 'NONE',  ( 29.98885399772409954, -6.604504582617394703, -4.533357778048668685 ) ) ;
#17060 = CARTESIAN_POINT ( 'NONE',  ( 27.57216386142120257, -6.895668018177890879, -7.033357778048666908 ) ) ;
#17062 = ADVANCED_FACE ( 'NONE', ( #16799 ), #111, .F. ) ;
#17061 = CARTESIAN_POINT ( 'NONE',  ( 13.34918303132433692, 14.15390528054681596, 16.46429318744779025 ) ) ;
#17063 = CARTESIAN_POINT ( 'NONE',  ( 12.50000000000000000, 1.530808498934191521E-15, -4.000000000000000000 ) ) ;
#17064 = CARTESIAN_POINT ( 'NONE',  ( -6.528882441595574626, 17.18907124314410950, 16.95629972507819971 ) ) ;
#17065 = CIRCLE ( 'NONE', #8946, 2.749999999999988454 ) ;
#17066 = VERTEX_POINT ( 'NONE', #14256 ) ;
#17067 = CARTESIAN_POINT ( 'NONE',  ( 28.23249303296521617, -2.754479417688857179, -4.705209693361161349 ) ) ;
#17068 = LINE ( 'NONE', #15695, #14205 ) ;
#17069 = CARTESIAN_POINT ( 'NONE',  ( -9.099998387031003944, -19.29508120620799616, 16.81964500401478091 ) ) ;
#17070 = CARTESIAN_POINT ( 'NONE',  ( 33.40660799972355477, 0.6401911282994665608, -5.783357778048661579 ) ) ;
#17071 = ADVANCED_FACE ( 'NONE', ( #5618 ), #1749, .F. ) ;
#17072 = LINE ( 'NONE', #13877, #10073 ) ;
#17073 = CARTESIAN_POINT ( 'NONE',  ( 29.18195272205665347, -2.340279496617377664, 7.033357778048666020 ) ) ;
#17074 = CARTESIAN_POINT ( 'NONE',  ( 26.23609683341064525, -2.995005734021441768, -6.861505862736159145 ) ) ;
#17075 = AXIS2_PLACEMENT_3D ( 'NONE', #2630, #4072, #16418 ) ;
#17076 = VERTEX_POINT ( 'NONE', #1654 ) ;
#17077 = FACE_BOUND ( 'NONE', #7880, .T. ) ;
#17078 = VERTEX_POINT ( 'NONE', #9879 ) ;
#17079 = CIRCLE ( 'NONE', #17682, 12.50000000000000000 ) ;
#17080 = CARTESIAN_POINT ( 'NONE',  ( 39.99999999999999289, 0.000000000000000000, 2.055000000000000160 ) ) ;
#17081 = DIRECTION ( 'NONE',  ( 1.000000000000000000, 0.000000000000000000, 0.000000000000000000 ) ) ;
#17082 = CARTESIAN_POINT ( 'NONE',  ( 25.76466184735054910, -2.811881907026620553, -6.248149982130924762 ) ) ;
#17083 = CARTESIAN_POINT ( 'NONE',  ( 26.53943449477818106, -2.321292140958837624, -6.453230759126469707 ) ) ;
#17084 = AXIS2_PLACEMENT_3D ( 'NONE', #8929, #954, #3935 ) ;
#17085 = CARTESIAN_POINT ( 'NONE',  ( 27.08121146544255353, -6.028038774645947839, -7.939653947423664704 ) ) ;
#17086 = ORIENTED_EDGE ( 'NONE', *, *, #3924, .T. ) ;
#17087 = FACE_OUTER_BOUND ( 'NONE', #5114, .T. ) ;
#17088 = CARTESIAN_POINT ( 'NONE',  ( 28.55151181693415907, -2.416235175459247486, -4.533357778048659803 ) ) ;
#17089 = DIRECTION ( 'NONE',  ( 0.000000000000000000, 0.000000000000000000, -1.000000000000000000 ) ) ;
#17090 = VERTEX_POINT ( 'NONE', #292 ) ;
#17091 = CARTESIAN_POINT ( 'NONE',  ( 30.54048978798443059, -6.538043363838207611, -4.533357778048668685 ) ) ;
#17092 = CIRCLE ( 'NONE', #16796, 2.749999999999988454 ) ;
#17093 = DIRECTION ( 'NONE',  ( -0.000000000000000000, -1.000000000000000000, -0.000000000000000000 ) ) ;
#17094 = CARTESIAN_POINT ( 'NONE',  ( 33.17094678975809074, -2.159493266760871499, 4.705209693361167567 ) ) ;
#17095 = EDGE_CURVE ( 'NONE', #9480, #7391, #11323, .T. ) ;
#17096 = ORIENTED_EDGE ( 'NONE', *, *, #2534, .T. ) ;
#17097 =( BOUNDED_CURVE ( )  B_SPLINE_CURVE ( 2, ( #2023, #10520, #13437, #2120, #9252, #11788, #14712, #17461, #2294 ),
 .UNSPECIFIED., .F., .T. ) 
 B_SPLINE_CURVE_WITH_KNOTS ( ( 3, 2, 2, 2, 3 ),
 ( 0.6730769230769231282, 0.6794871794871795156, 0.6923076923076922906, 0.7051282051282051766, 0.7115384615384615641 ),
 .UNSPECIFIED. ) 
 CURVE ( )  GEOMETRIC_REPRESENTATION_ITEM ( )  RATIONAL_B_SPLINE_CURVE ( ( 0.9330127018922192983, 0.9330127018922198534, 1.000000000000000000, 0.8660254037844387076, 1.000000000000000000, 0.8660254037844387076, 1.000000000000000000, 0.9330127018922194093, 0.9330127018922194093 ) ) 
 REPRESENTATION_ITEM ( '' )  );
#17098 = FACE_OUTER_BOUND ( 'NONE', #9612, .T. ) ;
#17099 = CARTESIAN_POINT ( 'NONE',  ( -17.22607755114822226, -18.63699807132245212, 15.96626374682043981 ) ) ;
#17100 = FACE_OUTER_BOUND ( 'NONE', #4602, .T. ) ;
#17101 = EDGE_LOOP ( 'NONE', ( #9149, #16937, #6909, #11192, #7639 ) ) ;
#17102 = LINE ( 'NONE', #4655, #3848 ) ;
#17103 = ORIENTED_EDGE ( 'NONE', *, *, #13539, .T. ) ;
#17104 = AXIS2_PLACEMENT_3D ( 'NONE', #9039, #11744, #16036 ) ;
#17105 = CARTESIAN_POINT ( 'NONE',  ( 8.632250723006720250, -18.84644399697197770, -16.84735068286506987 ) ) ;
#17106 = LINE ( 'NONE', #587, #17747 ) ;
#17107 = ORIENTED_EDGE ( 'NONE', *, *, #12652, .T. ) ;
#17108 = DIRECTION ( 'NONE',  ( -0.1196152422706610735, 0.9928203230275511881, 0.000000000000000000 ) ) ;
#17109 = CARTESIAN_POINT ( 'NONE',  ( 26.01652455409633902, -4.902371455920926380, -5.783357778048663356 ) ) ;
#17110 = CARTESIAN_POINT ( 'NONE',  ( -2.016448651773435938E-27, -20.49999999999999645, 13.00000000000000178 ) ) ;
#17111 = SHAPE_DEFINITION_REPRESENTATION ( #15193, #3339 ) ;
#17112 = DIRECTION ( 'NONE',  ( -1.000000000000000000, 0.000000000000000000, 0.000000000000000000 ) ) ;
#17113 = CARTESIAN_POINT ( 'NONE',  ( 32.30426898124760982, -6.025734024055190652, -6.861505862736167138 ) ) ;
#17114 = CARTESIAN_POINT ( 'NONE',  ( -9.749999999999953815, 3.897114317030088149, -3.000000000000000000 ) ) ;
#17115 = CARTESIAN_POINT ( 'NONE',  ( -29.25000000000000000, -16.21813761408365195, -13.37255996287876947 ) ) ;
#17116 = CARTESIAN_POINT ( 'NONE',  ( 30.43486631442457835, -6.877930660435475296, 5.783357778048657138 ) ) ;
#17117 = VECTOR ( 'NONE', #15889, 1000.000000000000000 ) ;
#17118 = EDGE_CURVE ( 'NONE', #4257, #16316, #11416, .T. ) ;
#17119 = EDGE_LOOP ( 'NONE', ( #5922, #14091, #12588, #15178, #5134, #13669, #8265, #14502, #17633, #10816, #10119, #3405, #13279, #9755, #5329, #8857, #1332, #6462, #509, #17579, #3525, #13336, #17789, #16261, #17454 ) ) ;
#17120 = LINE ( 'NONE', #15749, #988 ) ;
#17121 =( BOUNDED_CURVE ( )  B_SPLINE_CURVE ( 2, ( #14888, #13353, #5345, #6367, #1201, #17739, #9176, #2474, #10780 ),
 .UNSPECIFIED., .F., .T. ) 
 B_SPLINE_CURVE_WITH_KNOTS ( ( 3, 2, 2, 2, 3 ),
 ( 0.4038461538461538547, 0.4102564102564102422, 0.4230769230769230727, 0.4358974358974359031, 0.4423076923076923461 ),
 .UNSPECIFIED. ) 
 CURVE ( )  GEOMETRIC_REPRESENTATION_ITEM ( )  RATIONAL_B_SPLINE_CURVE ( ( 0.9330127018922194093, 0.9330127018922196314, 1.000000000000000000, 0.8660254037844387076, 1.000000000000000000, 0.8660254037844387076, 1.000000000000000000, 0.9330127018922190762, 0.9330127018922194093 ) ) 
 REPRESENTATION_ITEM ( '' )  );
#17122 = VERTEX_POINT ( 'NONE', #5959 ) ;
#17123 = CARTESIAN_POINT ( 'NONE',  ( 32.80318959510331212, -2.203800746085299522, 6.861505862736166250 ) ) ;
#17124 = CYLINDRICAL_SURFACE ( 'NONE', #11022, 2.499999999999999112 ) ;
#17125 = CARTESIAN_POINT ( 'NONE',  ( -7.499998387031003411, -20.49508120620799900, 6.000000000000000000 ) ) ;
#17126 = VECTOR ( 'NONE', #3304, 1000.000000000000000 ) ;
#17127 = EDGE_LOOP ( 'NONE', ( #12607, #797 ) ) ;
#17128 = CIRCLE ( 'NONE', #10990, 3.999999999999998224 ) ;
#17129 = CARTESIAN_POINT ( 'NONE',  ( -2.749999999999992895, -20.49999999999999645, -13.00000000000000178 ) ) ;
#17130 = CARTESIAN_POINT ( 'NONE',  ( -4.197477404309750249, 0.8522071663317478674, -3.205040426610024085 ) ) ;
#17131 = ORIENTED_EDGE ( 'NONE', *, *, #3407, .F. ) ;
#17132 = CARTESIAN_POINT ( 'NONE',  ( 29.16815758536418102, -2.004582921727632971, -5.783357778048664244 ) ) ;
#17133 = CARTESIAN_POINT ( 'NONE',  ( 32.83754810739938534, -9.116730809865837060, -4.216642221951339309 ) ) ;
#17134 = VECTOR ( 'NONE', #13230, 1000.000000000000000 ) ;
#17135 = CARTESIAN_POINT ( 'NONE',  ( 27.26436163736424945, -2.571311352887278190, -7.033357778048658027 ) ) ;
#17136 = DIRECTION ( 'NONE',  ( -0.000000000000000000, -0.000000000000000000, -1.000000000000000000 ) ) ;
#17137 = CARTESIAN_POINT ( 'NONE',  ( 4.211140560182196957, -2.431303136016550237, -3.445885042887436800 ) ) ;
#17138 = SURFACE_STYLE_USAGE ( .BOTH. , #11190 ) ;
#17139 = CARTESIAN_POINT ( 'NONE',  ( 26.87106449706838873, -6.053357334259913181, -3.627061608673667781 ) ) ;
#17140 =( BOUNDED_CURVE ( )  B_SPLINE_CURVE ( 2, ( #17035, #15662, #8779, #14312, #1895, #12935, #5673 ),
 .UNSPECIFIED., .F., .T. ) 
 B_SPLINE_CURVE_WITH_KNOTS ( ( 3, 2, 2, 3 ),
 ( 0.9423076923076922906, 0.9487179487179486781, 0.9615384615384615641, 0.9690340935984054216 ),
 .UNSPECIFIED. ) 
 CURVE ( )  GEOMETRIC_REPRESENTATION_ITEM ( )  RATIONAL_B_SPLINE_CURVE ( ( 0.9330127018922194093, 0.9330127018922194093, 1.000000000000000000, 0.8660254037844387076, 1.000000000000000000, 0.9216705062683109295, 0.9349331465915117212 ) ) 
 REPRESENTATION_ITEM ( '' )  );
#17141 = AXIS2_PLACEMENT_3D ( 'NONE', #827, #6358, #11880 ) ;
#17142 = CARTESIAN_POINT ( 'NONE',  ( 27.17934203385504333, -30.00000000000000355, 13.93658524716016878 ) ) ;
#17143 = CARTESIAN_POINT ( 'NONE',  ( 32.77701044293393551, -4.087866415376695706, 8.283357778048662468 ) ) ;
#17144 = EDGE_CURVE ( 'NONE', #15247, #17612, #14681, .T. ) ;
#17145 = ORIENTED_EDGE ( 'NONE', *, *, #6425, .T. ) ;
#17146 = AXIS2_PLACEMENT_3D ( 'NONE', #16706, #12702, #5804 ) ;
#17147 = ORIENTED_EDGE ( 'NONE', *, *, #13382, .T. ) ;
#17148 = CARTESIAN_POINT ( 'NONE',  ( 25.95642634701329499, -4.403549397486667516, 7.880302681851837576 ) ) ;
#17149 = CARTESIAN_POINT ( 'NONE',  ( 33.56062403295735663, -2.739515387291123982, 7.939653947423662927 ) ) ;
#17150 = SURFACE_STYLE_USAGE ( .BOTH. , #17336 ) ;
#17151 = CARTESIAN_POINT ( 'NONE',  ( -10.78415792467453471, 15.55827129984638901, -16.70145112110344598 ) ) ;
#17152 = DIRECTION ( 'NONE',  ( 0.1113444980252557837, 0.9937818688019538493, 0.000000000000000000 ) ) ;
#17154 = CIRCLE ( 'NONE', #6110, 5.000000000000000000 ) ;
#17153 = CARTESIAN_POINT ( 'NONE',  ( 30.78487334700428590, -1.819997462563214263, -5.783357778048658027 ) ) ;
#17155 = CARTESIAN_POINT ( 'NONE',  ( 31.05948030073166066, -1.776715885202022394, -5.783357778048662468 ) ) ;
#17156 = ADVANCED_FACE ( 'NONE', ( #8601 ), #2892, .F. ) ;
#17157 = CARTESIAN_POINT ( 'NONE',  ( 41.90164972253716513, -2.988527579590351646, -5.783357778048662468 ) ) ;
#17158 = ORIENTED_EDGE ( 'NONE', *, *, #13024, .F. ) ;
#17159 = CARTESIAN_POINT ( 'NONE',  ( -36.07773319708005744, -23.32620662758124297, 11.14818368178938357 ) ) ;
#17160 = CYLINDRICAL_SURFACE ( 'NONE', #7296, 6.249999999999996447 ) ;
#17161 = CARTESIAN_POINT ( 'NONE',  ( 26.16860980394290692, -3.430234601869349920, -3.283357778048662023 ) ) ;
#17162 = EDGE_LOOP ( 'NONE', ( #15578, #9166, #1524, #1832 ) ) ;
#17163 = CARTESIAN_POINT ( 'NONE',  ( 27.47505859511117521, -2.218764776483033163, -5.783357778048658027 ) ) ;
#17164 = DIRECTION ( 'NONE',  ( 0.9928203230275512992, 0.1196152422706610180, 4.006172263299093133E-17 ) ) ;
#17165 = CARTESIAN_POINT ( 'NONE',  ( 26.19644603989335963, -6.395740563884607432, -4.006386918492157889 ) ) ;
#17166 = CARTESIAN_POINT ( 'NONE',  ( 26.01652455409633902, -4.902371455920926380, -5.783357778048663356 ) ) ;
#17167 = CARTESIAN_POINT ( 'NONE',  ( 29.38468146192651886, -6.677295441714964142, 4.533357778048659803 ) ) ;
#17168 = ADVANCED_FACE ( 'NONE', ( #15584, #13957 ), #12771, .T. ) ;
#17169 = EDGE_LOOP ( 'NONE', ( #14388, #9396, #14525, #12211 ) ) ;
#17170 = CYLINDRICAL_SURFACE ( 'NONE', #14717, 2.499999999999999112 ) ;
#17171 = B_SPLINE_CURVE_WITH_KNOTS ( 'NONE', 1,
 ( #5093, #16273 ),
 .UNSPECIFIED., .F., .F.,
 ( 2, 2 ),
 ( 0.000000000000000000, 1.000000000000000000 ),
 .UNSPECIFIED. ) ;
#17172 = CARTESIAN_POINT ( 'NONE',  ( 31.91459173804835103, -5.445711903524953712, -3.627061608673667781 ) ) ;
#17173 = ORIENTED_EDGE ( 'NONE', *, *, #13260, .F. ) ;
#17174 = CIRCLE ( 'NONE', #2118, 0.9999999999999995559 ) ;
#17175 = LINE ( 'NONE', #3648, #5518 ) ;
#17176 = CARTESIAN_POINT ( 'NONE',  ( 25.88432464927661769, -3.805096980563277498, -7.814840548041910750 ) ) ;
#17177 = ORIENTED_EDGE ( 'NONE', *, *, #12068, .F. ) ;
#17178 = EDGE_CURVE ( 'NONE', #3121, #14370, #7948, .T. ) ;
#17179 = DIRECTION ( 'NONE',  ( 0.000000000000000000, 0.000000000000000000, -1.000000000000000000 ) ) ;
#17180 = CARTESIAN_POINT ( 'NONE',  ( 25.76326615456878244, -3.051972493152843580, -6.861505862736158257 ) ) ;
#17181 = AXIS2_PLACEMENT_3D ( 'NONE', #14283, #8922, #14462 ) ;
#17182 = CARTESIAN_POINT ( 'NONE',  ( 26.45077056032005913, -6.103994453487816330, -7.939653947423664704 ) ) ;
#17183 = DIRECTION ( 'NONE',  ( 0.000000000000000000, 1.000000000000000000, 0.000000000000000000 ) ) ;
#17184 = CARTESIAN_POINT ( 'NONE',  ( 33.81344892038539740, -6.481075040654872943, -6.453230759126470595 ) ) ;
#17185 = VECTOR ( 'NONE', #10475, 1000.000000000000000 ) ;
#17186 = DIRECTION ( 'NONE',  ( -0.000000000000000000, -1.000000000000000000, -0.000000000000000000 ) ) ;
#17187 = CARTESIAN_POINT ( 'NONE',  ( 29.07687923786957285, -2.352938776424351008, -7.033357778048658027 ) ) ;
#17188 = B_SPLINE_CURVE_WITH_KNOTS ( 'NONE', 1,
 ( #1911, #1637 ),
 .UNSPECIFIED., .F., .F.,
 ( 2, 2 ),
 ( 0.000000000000000000, 1.000000000000000000 ),
 .UNSPECIFIED. ) ;
#17189 = CARTESIAN_POINT ( 'NONE',  ( -16.75000000000000000, -16.21813761408365195, 13.00000000000000178 ) ) ;
#17190 = CARTESIAN_POINT ( 'NONE',  ( 33.27602027394517847, -2.146833986953896822, 6.861505862736165362 ) ) ;
#17191 = EDGE_CURVE ( 'NONE', #1012, #14557, #11640, .T. ) ;
#17192 = VERTEX_POINT ( 'NONE', #16773 ) ;
#17193 = CIRCLE ( 'NONE', #14276, 0.9000000000000003553 ) ;
#17194 = ORIENTED_EDGE ( 'NONE', *, *, #12597, .F. ) ;
#17195 = DIRECTION ( 'NONE',  ( -1.000000000000000000, 0.000000000000000000, 0.000000000000000000 ) ) ;
#17196 = CARTESIAN_POINT ( 'NONE',  ( -15.92260893619738837, -28.39189527176317540, -16.15082599432113142 ) ) ;
#17197 = CARTESIAN_POINT ( 'NONE',  ( 28.01872616749444944, -6.841866079205687790, 7.033357778048657138 ) ) ;
#17198 = EDGE_CURVE ( 'NONE', #17749, #11286, #1724, .T. ) ;
#17199 = ORIENTED_EDGE ( 'NONE', *, *, #10886, .F. ) ;
#17200 = CARTESIAN_POINT ( 'NONE',  ( 33.86058074732183343, -3.957317592522819005, -3.455209693361164902 ) ) ;
#17201 = VERTEX_POINT ( 'NONE', #11399 ) ;
#17202 = CARTESIAN_POINT ( 'NONE',  ( 25.76466184735054910, -2.811881907026620553, -6.248149982130924762 ) ) ;
#17203 = CARTESIAN_POINT ( 'NONE',  ( 26.25597102934084859, -6.889804849753313754, -7.289619350601861392 ) ) ;
#17204 = CARTESIAN_POINT ( 'NONE',  ( 33.95908713831674675, -3.945449517755637903, -5.783357778048663356 ) ) ;
#17205 = EDGE_CURVE ( 'NONE', #12240, #14461, #7353, .T. ) ;
#17206 = CARTESIAN_POINT ( 'NONE',  ( 29.15568435273173264, -2.343444316361667834, -7.033357778048658027 ) ) ;
#17207 = CIRCLE ( 'NONE', #17516, 3.999999999999999112 ) ;
#17208 = CARTESIAN_POINT ( 'NONE',  ( -1.500000000000000666, -5.809475019311125976, -2.000000000000000000 ) ) ;
#17209 = ITEM_DEFINED_TRANSFORMATION ( 'NONE', 'NONE', #4751,  #3575 ) ;
#17210 = DIRECTION ( 'NONE',  ( -0.1196152422706610041, 0.9928203230275510771, 0.000000000000000000 ) ) ;
#17211 = B_SPLINE_CURVE_WITH_KNOTS ( 'NONE', 3,
 ( #1360, #5333, #17894, #2637 ),
 .UNSPECIFIED., .F., .F.,
 ( 4, 4 ),
 ( 2.843119637683901301E-07, 0.001422633878257846193 ),
 .UNSPECIFIED. ) ;
#17212 = CARTESIAN_POINT ( 'NONE',  ( 33.54323074294813267, -5.249493066516778050, -7.939653947423664704 ) ) ;
#17213 = DIRECTION ( 'NONE',  ( 0.9928203230275512992, 0.1196152422706610180, 4.006172263299093133E-17 ) ) ;
#17214 = VECTOR ( 'NONE', #390, 1000.000000000000227 ) ;
#17215 = CARTESIAN_POINT ( 'NONE',  ( 28.52162355051263987, -6.481468097106410475, 4.705209693361159573 ) ) ;
#17216 = ORIENTED_EDGE ( 'NONE', *, *, #14425, .T. ) ;
#17217 =( BOUNDED_CURVE ( )  B_SPLINE_CURVE ( 3, ( #12083, #10460, #9451, #10544 ),
 .UNSPECIFIED., .F., .T. ) 
 B_SPLINE_CURVE_WITH_KNOTS ( ( 4, 4 ),
 ( 4.774018107371971631, 4.846194975958193929 ),
 .UNSPECIFIED. ) 
 CURVE ( )  GEOMETRIC_REPRESENTATION_ITEM ( )  RATIONAL_B_SPLINE_CURVE ( ( 1.000000000000000000, 0.9995659220841806025, 0.9995659220841806025, 1.000000000000000000 ) ) 
 REPRESENTATION_ITEM ( '' )  );
#17218 = ORIENTED_EDGE ( 'NONE', *, *, #829, .F. ) ;
#17219 = CARTESIAN_POINT ( 'NONE',  ( 26.86653773853314320, -2.919050055179571945, -6.861505862736159145 ) ) ;
#17220 = ORIENTED_EDGE ( 'NONE', *, *, #5162, .F. ) ;
#17221 = CARTESIAN_POINT ( 'NONE',  ( 33.56515079149260572, -5.873822666371450119, 4.705209693361159573 ) ) ;
#17222 = CARTESIAN_POINT ( 'NONE',  ( 14.00000000000000178, -1.714505518806294835E-15, 10.50000000000000000 ) ) ;
#17223 = CARTESIAN_POINT ( 'NONE',  ( 26.31556265977298992, -7.384422263489805793, 5.783357778048663356 ) ) ;
#17224 = EDGE_LOOP ( 'NONE', ( #4959, #4631, #14835, #7011, #5678, #6508 ) ) ;
#17225 = DIRECTION ( 'NONE',  ( -0.000000000000000000, -0.000000000000000000, -1.000000000000000000 ) ) ;
#17226 = DIRECTION ( 'NONE',  ( -0.1035898384862230653, 0.8598076211353318232, -0.4999999999999999445 ) ) ;
#17227 = ADVANCED_BREP_SHAPE_REPRESENTATION ( '', ( #11368, #3575 ), #2991 ) ;
#17228 = ORIENTED_EDGE ( 'NONE', *, *, #13511, .F. ) ;
#17229 = CARTESIAN_POINT ( 'NONE',  ( 2.449848172108562316, 3.432307619358737849, -3.203702292528906259 ) ) ;
#17230 = DIRECTION ( 'NONE',  ( 0.000000000000000000, -0.4999999999999991118, 0.8660254037844390407 ) ) ;
#17231 = CARTESIAN_POINT ( 'NONE',  ( 26.60013260893011378, -1.924431040879551746, -5.783357778048658027 ) ) ;
#17232 = EDGE_CURVE ( 'NONE', #11951, #15953, #14233, .T. ) ;
#17233 = PLANE ( 'NONE',  #4305 ) ;
#17234 = DIRECTION ( 'NONE',  ( -0.000000000000000000, -0.000000000000000000, -1.000000000000000000 ) ) ;
#17235 = FILL_AREA_STYLE ('',( #11667 ) ) ;
#17236 = CARTESIAN_POINT ( 'NONE',  ( 28.99445422935450267, -6.424501337975009996, -6.861505862736166250 ) ) ;
#17237 = CARTESIAN_POINT ( 'NONE',  ( 27.93543013035303701, -2.153102235610331316, 6.453230759126468818 ) ) ;
#17238 = CARTESIAN_POINT ( 'NONE',  ( 31.01321894478757812, -1.392741288986461212, 5.783357778048668685 ) ) ;
#17239 =( BOUNDED_CURVE ( )  B_SPLINE_CURVE ( 2, ( #4965, #17149, #537, #15680, #3260, #7698, #8795, #6332, #13224, #10403, #895, #11761, #3435, #717, #9057, #14328, #11854, #628, #6154, #6242, #17334, #4697, #11677, #7522, #17433, #10226, #3524, #8964, #801, #16055, #15772, #10495, #3624, #9148, #14686, #2267, #2091, #1910, #7433, #17247, #16141, #10836, #1337, #991, #16227, #7965, #7879, #3797, #9316, #3885, #14855, #17616, #13498, #13411, #5136, #17874, #2519, #8044, #17703, #6518, #12309, #2443, #2612, #9566, #5224, #12030, #12387, #1072, #16401, #10655, #9399, #10745, #6594, #12124, #14773, #8226, #5397, #16321, #14941, #13757, #15023, #13582, #1164, #6683, #12218, #17793, #6861, #5313, #3969, #9484, #9226, #1260, #8140, #13670, #15116, #6776, #10915, #16483, #4055, #2703, #2360, #5055, #10574, #3701, #7331, #15289, #5757, #13836, #4323, #153, #11096, #1425, #9653, #3145, #7234, #11177, #8308, #8681, #9928, #12571, #2870, #9734, #246, #4155, #8397, #15203, #14115, #5488, #7146, #6948, #12481, #12657, #2785, #15563, #11272, #67, #14206, #5579, #16944, #15477, #16662, #4501, #16849, #14028, #16750, #4414, #1800, #15384, #4235 ),
 .UNSPECIFIED., .F., .T. ) 
 B_SPLINE_CURVE_WITH_KNOTS ( ( 3, 2, 2, 2, 2, 2, 2, 2, 2, 2, 2, 2, 2, 2, 2, 2, 2, 2, 2, 2, 2, 2, 2, 2, 2, 2, 2, 2, 2, 2, 2, 2, 2, 2, 2, 2, 2, 2, 2, 2, 2, 2, 2, 2, 2, 2, 2, 2, 2, 2, 2, 2, 2, 2, 2, 2, 2, 2, 2, 2, 2, 2, 2, 2, 2, 2, 2, 2, 2, 2, 2, 2, 2, 2, 3 ),
 ( 0.000000000000000000, 0.01322951878407230102, 0.02645903756814460203, 0.03968855635221691519, 0.05291807513628920406, 0.06614759392036151375, 0.07937711270443383038, 0.09260663148850611925, 0.1058361502725784081, 0.1190656690566507248, 0.1322951878407230275, 0.1455247066247953303, 0.1587542254088676608, 0.1719837441929399358, 0.1852132629770122385, 0.1984427817610845690, 0.2116723005451568163, 0.2249018193292291468, 0.2381313381133014495, 0.2513608568973737523, 0.2645903756814460550, 0.2778198944655183578, 0.2910494132495906605, 0.3042789320336629633, 0.3175084508177353215, 0.3307379696018076243, 0.3439674883858798715, 0.3571970071699521743, 0.3704265259540244770, 0.3836560447380968353, 0.3968855635221691380, 0.4101150823062413853, 0.4233446010903136325, 0.4365741198743859908, 0.4498036386584582935, 0.4630331574425305963, 0.4762626762266028990, 0.4894921950106752018, 0.5027217137947475045, 0.5159512325788198073, 0.5291807513628921100, 0.5424102701469644128, 0.5556397889310367155, 0.5688693077151090183, 0.5820988264991813210, 0.5953283452832536238, 0.6085578640673259265, 0.6217873828513982293, 0.6350169016354706431, 0.6482464204195428348, 0.6614759392036152486, 0.6747054579876874403, 0.6879349767717597430, 0.7011644955558321568, 0.7143940143399043485, 0.7276235331239767623, 0.7408530519080489540, 0.7540825706921212568, 0.7673120894761936706, 0.7805416082602658623, 0.7937711270443382761, 0.8070006458284105788, 0.8202301646124827705, 0.8334596833965551843, 0.8466892021806272650, 0.8599187209646996788, 0.8731482397487719815, 0.8863777585328441733, 0.8996072773169165870, 0.9128367961009887788, 0.9260663148850611925, 0.9392958336691334953, 0.9525253524532057980, 0.9657548712372781008, 0.9750618896629086318 ),
 .UNSPECIFIED. ) 
 CURVE ( )  GEOMETRIC_REPRESENTATION_ITEM ( )  RATIONAL_B_SPLINE_CURVE ( ( 1.000000000000000000, 0.8660254037844387076, 1.000000000000000000, 0.8660254037844387076, 1.000000000000000000, 0.8660254037844387076, 1.000000000000000000, 0.8660254037844387076, 1.000000000000000000, 0.8660254037844387076, 1.000000000000000000, 0.8660254037844387076, 1.000000000000000000, 0.8660254037844387076, 1.000000000000000000, 0.8660254037844387076, 1.000000000000000000, 0.8660254037844387076, 1.000000000000000000, 0.8660254037844387076, 1.000000000000000000, 0.8660254037844387076, 1.000000000000000000, 0.8660254037844387076, 1.000000000000000000, 0.8660254037844387076, 1.000000000000000000, 0.8660254037844387076, 1.000000000000000000, 0.8660254037844387076, 1.000000000000000000, 0.8660254037844387076, 1.000000000000000000, 0.8660254037844387076, 1.000000000000000000, 0.8660254037844387076, 1.000000000000000000, 0.8660254037844387076, 1.000000000000000000, 0.8660254037844387076, 1.000000000000000000, 0.8660254037844387076, 1.000000000000000000, 0.8660254037844387076, 1.000000000000000000, 0.8660254037844387076, 1.000000000000000000, 0.8660254037844387076, 1.000000000000000000, 0.8660254037844387076, 1.000000000000000000, 0.8660254037844387076, 1.000000000000000000, 0.8660254037844387076, 1.000000000000000000, 0.8660254037844387076, 1.000000000000000000, 0.8660254037844387076, 1.000000000000000000, 0.8660254037844387076, 1.000000000000000000, 0.8660254037844387076, 1.000000000000000000, 0.8660254037844387076, 1.000000000000000000, 0.8660254037844387076, 1.000000000000000000, 0.8660254037844387076, 1.000000000000000000, 0.8660254037844387076, 1.000000000000000000, 0.8660254037844387076, 1.000000000000000000, 0.8660254037844387076, 1.000000000000000000, 0.8660254037844387076, 1.000000000000000000, 0.8660254037844387076, 1.000000000000000000, 0.8660254037844387076, 1.000000000000000000, 0.8660254037844387076, 1.000000000000000000, 0.8660254037844387076, 1.000000000000000000, 0.8660254037844387076, 1.000000000000000000, 0.8660254037844387076, 1.000000000000000000, 0.8660254037844387076, 1.000000000000000000, 0.8660254037844387076, 1.000000000000000000, 0.8660254037844387076, 1.000000000000000000, 0.8660254037844387076, 1.000000000000000000, 0.8660254037844387076, 1.000000000000000000, 0.8660254037844387076, 1.000000000000000000, 0.8660254037844387076, 1.000000000000000000, 0.8660254037844387076, 1.000000000000000000, 0.8660254037844387076, 1.000000000000000000, 0.8660254037844387076, 1.000000000000000000, 0.8660254037844387076, 1.000000000000000000, 0.8660254037844387076, 1.000000000000000000, 0.8660254037844387076, 1.000000000000000000, 0.8660254037844387076, 1.000000000000000000, 0.8660254037844387076, 1.000000000000000000, 0.8660254037844387076, 1.000000000000000000, 0.8660254037844387076, 1.000000000000000000, 0.8660254037844387076, 1.000000000000000000, 0.8660254037844387076, 1.000000000000000000, 0.8660254037844387076, 1.000000000000000000, 0.8660254037844387076, 1.000000000000000000, 0.8660254037844387076, 1.000000000000000000, 0.8660254037844387076, 1.000000000000000000, 0.8660254037844387076, 1.000000000000000000, 0.8660254037844387076, 1.000000000000000000, 0.8660254037844387076, 1.000000000000000000, 0.8660254037844387076, 1.000000000000000000, 0.8660254037844387076, 1.000000000000000000, 0.8660254037844387076, 1.000000000000000000, 0.9057483453558528019, 0.9441095091726994237 ) ) 
 REPRESENTATION_ITEM ( '' )  );
#17240 = EDGE_CURVE ( 'NONE', #13718, #14027, #3789, .T. ) ;
#17241 = EDGE_LOOP ( 'NONE', ( #1634, #2586, #3745, #6196 ) ) ;
#17242 = ORIENTED_EDGE ( 'NONE', *, *, #10260, .F. ) ;
#17243 = VERTEX_POINT ( 'NONE', #4873 ) ;
#17244 =( GEOMETRIC_REPRESENTATION_CONTEXT ( 3 ) GLOBAL_UNCERTAINTY_ASSIGNED_CONTEXT ( ( #16066 ) ) GLOBAL_UNIT_ASSIGNED_CONTEXT ( ( #3046, #11165, #4572 ) ) REPRESENTATION_CONTEXT ( 'NONE', 'WORKASPACE' ) );
#17245 = EDGE_LOOP ( 'NONE', ( #13931, #1233, #16562, #15706, #10988, #5558, #15168, #16448, #15351, #5982, #15579 ) ) ;
#17246 = CARTESIAN_POINT ( 'NONE',  ( 26.49461065740898391, -7.352653653197164907, 5.783357778048658915 ) ) ;
#17247 = CARTESIAN_POINT ( 'NONE',  ( 31.41531425212677675, -1.744041783721344219, 5.783357778048668685 ) ) ;
#17248 = CARTESIAN_POINT ( 'NONE',  ( -10.50000000000000000, 0.000000000000000000, -2.000000000000000000 ) ) ;
#17249 = CARTESIAN_POINT ( 'NONE',  ( -17.83875296969244673, 10.53491135297441161, -15.87472302800564350 ) ) ;
#17250 = CARTESIAN_POINT ( 'NONE',  ( -27.68843801662522353, -20.37088413741627235, -13.80304640004047023 ) ) ;
#17251 = CARTESIAN_POINT ( 'NONE',  ( 32.28234893270314387, -5.401404424200516807, -7.939653947423664704 ) ) ;
#17252 = LINE ( 'NONE', #3532, #12483 ) ;
#17253 = CARTESIAN_POINT ( 'NONE',  ( 2.500000000000000000, 1.768423874527825124, 1.020999999999998797 ) ) ;
#17254 = CYLINDRICAL_SURFACE ( 'NONE', #11626, 5.000000000000000000 ) ;
#17255 = CARTESIAN_POINT ( 'NONE',  ( 31.08079519141086067, -2.838413270685653078, -8.283357778048660691 ) ) ;
#17256 = EDGE_CURVE ( 'NONE', #6312, #15379, #14002, .T. ) ;
#17257 = DIRECTION ( 'NONE',  ( 1.000000000000000000, 0.000000000000000000, 0.000000000000000000 ) ) ;
#17258 = VERTEX_POINT ( 'NONE', #17535 ) ;
#17259 = EDGE_LOOP ( 'NONE', ( #5661, #9814, #8471, #11651 ) ) ;
#17260 = CARTESIAN_POINT ( 'NONE',  ( 33.56062403295735663, -2.739515387291124426, -3.627061608673662008 ) ) ;
#17261 = CYLINDRICAL_SURFACE ( 'NONE', #15069, 2.749999999999992895 ) ;
#17262 = VERTEX_POINT ( 'NONE', #10130 ) ;
#17263 = CARTESIAN_POINT ( 'NONE',  ( 26.31556265977298992, -7.384422263489805793, 5.783357778048663356 ) ) ;
#17264 = CARTESIAN_POINT ( 'NONE',  ( 27.42949161418789572, -3.278323244185609830, 8.283357778048664244 ) ) ;
#17265 = ORIENTED_EDGE ( 'NONE', *, *, #7690, .T. ) ;
#17266 = CARTESIAN_POINT ( 'NONE',  ( 29.37220822929407760, -7.016156836349003001, -5.783357778048668685 ) ) ;
#17267 = CARTESIAN_POINT ( 'NONE',  ( 32.12473870642251939, -5.420393343910986594, -7.939653947423662927 ) ) ;
#17268 = VERTEX_POINT ( 'NONE', #13317 ) ;
#17269 = CARTESIAN_POINT ( 'NONE',  ( 29.47916769939009285, -7.003270332485284300, -6.453230759126468818 ) ) ;
#17270 = B_SPLINE_CURVE_WITH_KNOTS ( 'NONE', 3,
 ( #9863, #15418, #3271, #5883, #7087, #1644 ),
 .UNSPECIFIED., .F., .F.,
 ( 4, 2, 4 ),
 ( 0.002365888236227972966, 0.003551327329835079344, 0.004736766423442184855 ),
 .UNSPECIFIED. ) ;
#17271 = CARTESIAN_POINT ( 'NONE',  ( 31.29168529989541270, -6.784897756022354010, -6.453230759126470595 ) ) ;
#17272 = CYLINDRICAL_SURFACE ( 'NONE', #10979, 2.749999999999992006 ) ;
#17273 = DIRECTION ( 'NONE',  ( 0.9928203230275512992, 0.1196152422706610180, 4.006172263299093133E-17 ) ) ;
#17274 = AXIS2_PLACEMENT_3D ( 'NONE', #9468, #16469, #10901 ) ;
#17275 = ADVANCED_FACE ( 'NONE', ( #13138 ), #15956, .T. ) ;
#17276 = CARTESIAN_POINT ( 'NONE',  ( 27.12505156253147476, -7.276697974355294640, -5.783357778048668685 ) ) ;
#17277 = CARTESIAN_POINT ( 'NONE',  ( 28.12379965168153362, -6.829206799398704675, -7.033357778048666908 ) ) ;
#17278 = CARTESIAN_POINT ( 'NONE',  ( -8.776279441628744848, 6.799038105676760146, -2.000000000000000000 ) ) ;
#17279 = CARTESIAN_POINT ( 'NONE',  ( 7.499998387031003411, -20.49508120620799900, -13.00000000000000178 ) ) ;
#17280 = CARTESIAN_POINT ( 'NONE',  ( 29.77118727536320719, -5.903822331637461396, -3.283357778048667797 ) ) ;
#17281 = CARTESIAN_POINT ( 'NONE',  ( -23.00000000000000000, -16.21813761408365195, 13.00000000000000178 ) ) ;
#17282 = EDGE_CURVE ( 'NONE', #13969, #8628, #16906, .T. ) ;
#17283 = CARTESIAN_POINT ( 'NONE',  ( 31.41114436565740320, -6.133337902414513820, 6.861505862736158257 ) ) ;
#17284 = ORIENTED_EDGE ( 'NONE', *, *, #1084, .F. ) ;
#17285 = DIRECTION ( 'NONE',  ( 1.000000000000000000, 0.000000000000000000, 0.000000000000000000 ) ) ;
#17286 = DIRECTION ( 'NONE',  ( 0.8243186046180107640, -0.5661261679878571984, 0.000000000000000000 ) ) ;
#17287 = CARTESIAN_POINT ( 'NONE',  ( 27.42949161418789217, -3.278323244185609830, 8.283357778048666020 ) ) ;
#17288 = ORIENTED_EDGE ( 'NONE', *, *, #16362, .T. ) ;
#17289 = CARTESIAN_POINT ( 'NONE',  ( 2.500000000000000000, -1.178949249685218081, -2.041999999999998039 ) ) ;
#17290 = DIRECTION ( 'NONE',  ( 0.000000000000000000, 3.469446951953614189E-16, 1.000000000000000000 ) ) ;
#17291 = CARTESIAN_POINT ( 'NONE',  ( 25.94006848055682113, -4.267777217026356595, -3.719179227265282162 ) ) ;
#17292 = CARTESIAN_POINT ( 'NONE',  ( 3.248936832696173393, 17.78798921770683350, -17.00000000000000000 ) ) ;
#17293 = CARTESIAN_POINT ( 'NONE',  ( -7.499998387031003411, -20.49508120620799900, 12.00000000000000000 ) ) ;
#17294 = ORIENTED_EDGE ( 'NONE', *, *, #16630, .F. ) ;
#17295 = EDGE_CURVE ( 'NONE', #17243, #6446, #7615, .T. ) ;
#17296 = CARTESIAN_POINT ( 'NONE',  ( 30.57046727500519978, -4.353711291323232757, -8.283357778048662468 ) ) ;
#17297 = DIRECTION ( 'NONE',  ( 0.000000000000000000, 0.000000000000000000, -1.000000000000000000 ) ) ;
#17298 = ITEM_DEFINED_TRANSFORMATION ( 'NONE', 'NONE', #12573,  #3575 ) ;
#17299 = FACE_OUTER_BOUND ( 'NONE', #5295, .T. ) ;
#17300 = CARTESIAN_POINT ( 'NONE',  ( 29.97942892559193950, -4.424919740341219487, -3.627061608673664672 ) ) ;
#17301 = DIRECTION ( 'NONE',  ( -0.000000000000000000, -0.000000000000000000, 1.000000000000000000 ) ) ;
#17302 = CARTESIAN_POINT ( 'NONE',  ( 33.95908713831673964, -3.945449517755637014, -5.783357778048663356 ) ) ;
#17303 = EDGE_CURVE ( 'NONE', #14701, #3274, #17239, .T. ) ;
#17304 = CARTESIAN_POINT ( 'NONE',  ( 28.26310972651430120, -2.123820177930694442, 5.783357778048668685 ) ) ;
#17305 = ORIENTED_EDGE ( 'NONE', *, *, #4330, .T. ) ;
#17306 = EDGE_CURVE ( 'NONE', #14000, #11482, #5377, .T. ) ;
#17307 = ORIENTED_EDGE ( 'NONE', *, *, #16354, .T. ) ;
#17308 = CARTESIAN_POINT ( 'NONE',  ( 25.81099976294218479, -6.186279776075334524, -7.540300355390971987 ) ) ;
#17309 = ORIENTED_EDGE ( 'NONE', *, *, #7263, .F. ) ;
#17310 = CARTESIAN_POINT ( 'NONE',  ( 31.87075164095941915, -4.197052703815608687, 7.939653947423662039 ) ) ;
#17311 = CARTESIAN_POINT ( 'NONE',  ( -26.79938379600875109, -11.23877132507977805, 14.03531701109484331 ) ) ;
#17312 = CARTESIAN_POINT ( 'NONE',  ( -3.349226789952655547, -2.685125164760741256, -0.2236248678334855911 ) ) ;
#17313 = VERTEX_POINT ( 'NONE', #8494 ) ;
#17314 = CARTESIAN_POINT ( 'NONE',  ( 0.000000000000000000, 0.000000000000000000, 2.399999999999999467 ) ) ;
#17315 = CARTESIAN_POINT ( 'NONE',  ( 33.95908713831674675, -3.945449517755637903, 5.783357778048663356 ) ) ;
#17316 = CARTESIAN_POINT ( 'NONE',  ( 32.04575515724926760, -1.668086104879473730, -5.783357778048658027 ) ) ;
#17317 = CARTESIAN_POINT ( 'NONE',  ( 30.64918316926811315, -2.463315982128351678, -6.861505862736159145 ) ) ;
#17318 = CARTESIAN_POINT ( 'NONE',  ( 25.11802603177690330, -16.03270077640482683, 10.53798182577225084 ) ) ;
#17319 = FACE_OUTER_BOUND ( 'NONE', #9258, .T. ) ;
#17320 = FILL_AREA_STYLE ('',( #5043 ) ) ;
#17321 = CARTESIAN_POINT ( 'NONE',  ( 27.47505859511117521, -2.218764776483033163, -5.783357778048658027 ) ) ;
#17322 =( BOUNDED_CURVE ( )  B_SPLINE_CURVE ( 2, ( #11586, #902, #10500, #2001, #17539, #3352, #7620, #16061, #9153 ),
 .UNSPECIFIED., .F., .T. ) 
 B_SPLINE_CURVE_WITH_KNOTS ( ( 3, 2, 2, 2, 3 ),
 ( 0.4038461538461538547, 0.4102564102564102422, 0.4230769230769230727, 0.4358974358974359031, 0.4423076923076923461 ),
 .UNSPECIFIED. ) 
 CURVE ( )  GEOMETRIC_REPRESENTATION_ITEM ( )  RATIONAL_B_SPLINE_CURVE ( ( 0.9330127018922194093, 0.9330127018922196314, 1.000000000000000000, 0.8660254037844387076, 1.000000000000000000, 0.8660254037844387076, 1.000000000000000000, 0.9330127018922190762, 0.9330127018922194093 ) ) 
 REPRESENTATION_ITEM ( '' )  );
#17323 = AXIS2_PLACEMENT_3D ( 'NONE', #8535, #17398, #10798 ) ;
#17324 = DIRECTION ( 'NONE',  ( 0.000000000000000000, 1.224646799147353207E-16, 1.000000000000000000 ) ) ;
#17325 = MANIFOLD_SOLID_BREP ( 'Hex', #312 ) ;
#17326 = CARTESIAN_POINT ( 'NONE',  ( 30.03006034954003667, -2.965006068755446478, 8.283357778048664244 ) ) ;
#17327 = VERTEX_POINT ( 'NONE', #7419 ) ;
#17328 = ORIENTED_EDGE ( 'NONE', *, *, #8089, .F. ) ;
#17329 = VECTOR ( 'NONE', #17526, 1000.000000000000000 ) ;
#17330 = ORIENTED_EDGE ( 'NONE', *, *, #578, .T. ) ;
#17331 = VERTEX_POINT ( 'NONE', #13022 ) ;
#17332 = ADVANCED_FACE ( 'NONE', ( #1892 ), #8580, .T. ) ;
#17333 = CARTESIAN_POINT ( 'NONE',  ( 26.59574320524588842, -2.314508053356755024, 6.453230759126468818 ) ) ;
#17334 = CARTESIAN_POINT ( 'NONE',  ( 32.93470988637010066, -5.949778345213319497, 4.705209693361159573 ) ) ;
#17335 = ORIENTED_EDGE ( 'NONE', *, *, #9303, .T. ) ;
#17336 = SURFACE_SIDE_STYLE ('',( #6520 ) ) ;
#17337 = VECTOR ( 'NONE', #12906, 1000.000000000000000 ) ;
#17338 = CARTESIAN_POINT ( 'NONE',  ( 0.000000000000000000, 0.000000000000000000, -10.50000000000000000 ) ) ;
#17339 = CARTESIAN_POINT ( 'NONE',  ( -25.76436512043297711, -21.83811057962065405, -14.29411090273705831 ) ) ;
#17340 = CARTESIAN_POINT ( 'NONE',  ( 27.67650891848073158, -3.448435056481901295, -7.939653947423660263 ) ) ;
#17341 = CARTESIAN_POINT ( 'NONE',  ( 31.20090818012769773, -4.277755612481361602, -8.283357778048662468 ) ) ;
#17342 = FACE_OUTER_BOUND ( 'NONE', #10630, .T. ) ;
#17343 = DIRECTION ( 'NONE',  ( 0.9928203230275510771, 0.1196152422706610596, 9.614813431917826478E-17 ) ) ;
#17344 = CARTESIAN_POINT ( 'NONE',  ( 38.15053902264412500, -1.114360604510108876, -1.783357778048662912 ) ) ;
#17345 = UNCERTAINTY_MEASURE_WITH_UNIT (LENGTH_MEASURE( 1.000000000000000082E-05 ), #1812, 'distance_accuracy_value', 'NONE');
#17346 = CARTESIAN_POINT ( 'NONE',  ( 30.03080348965042745, -6.936809113706096319, -6.453230759126468818 ) ) ;
#17347 = DIRECTION ( 'NONE',  ( 1.000000000000000000, 0.000000000000000000, 0.000000000000000000 ) ) ;
#17348 = ORIENTED_EDGE ( 'NONE', *, *, #7732, .T. ) ;
#17349 = CARTESIAN_POINT ( 'NONE',  ( 27.73357241910951743, -6.576412695658750529, -6.861505862736166250 ) ) ;
#17350 = CARTESIAN_POINT ( 'NONE',  ( 32.07220196432898263, -5.426722983814484813, -3.627061608673668225 ) ) ;
#17351 = ORIENTED_EDGE ( 'NONE', *, *, #6273, .T. ) ;
#17352 = CARTESIAN_POINT ( 'NONE',  ( 3.355112389629170355, -2.681727112203166730, -0.2256878752776763641 ) ) ;
#17353 = CIRCLE ( 'NONE', #16752, 6.000000000000000888 ) ;
#17354 = CARTESIAN_POINT ( 'NONE',  ( -25.74999999999999289, -16.21813761408365195, -13.00000000000000178 ) ) ;
#17355 = CIRCLE ( 'NONE', #820, 2.749999999999991118 ) ;
#17356 = APPLICATION_CONTEXT ( 'automotive_design' ) ;
#17357 = ORIENTED_EDGE ( 'NONE', *, *, #9303, .F. ) ;
#17358 = EDGE_CURVE ( 'NONE', #11446, #11147, #10239, .T. ) ;
#17359 = B_SPLINE_CURVE_WITH_KNOTS ( 'NONE', 3,
 ( #2325, #13370, #6485, #1961 ),
 .UNSPECIFIED., .F., .F.,
 ( 4, 4 ),
 ( 0.000000000000000000, 0.0003446252387907819490 ),
 .UNSPECIFIED. ) ;
#17360 = CARTESIAN_POINT ( 'NONE',  ( 29.11066736118121767, -3.075774767273946608, -8.283357778048660691 ) ) ;
#17361 = ADVANCED_FACE ( 'NONE', ( #6030 ), #10380, .F. ) ;
#17362 = AXIS2_PLACEMENT_3D ( 'NONE', #10589, #14871, #14954 ) ;
#17363 = CARTESIAN_POINT ( 'NONE',  ( 31.91006497951310550, -2.311404624444611589, -6.861505862736159145 ) ) ;
#17364 = ORIENTED_EDGE ( 'NONE', *, *, #10152, .F. ) ;
#17365 = DIRECTION ( 'NONE',  ( 0.000000000000000000, 0.000000000000000000, 1.000000000000000000 ) ) ;
#17366 = DIRECTION ( 'NONE',  ( -0.000000000000000000, 1.000000000000000000, -0.000000000000000000 ) ) ;
#17367 = ORIENTED_EDGE ( 'NONE', *, *, #17144, .F. ) ;
#17368 = VECTOR ( 'NONE', #14761, 1000.000000000000114 ) ;
#17369 = CARTESIAN_POINT ( 'NONE',  ( 4.141042022537587464, -2.227970427079385640, -3.387027626239166089 ) ) ;
#17370 = AXIS2_PLACEMENT_3D ( 'NONE', #58, #17945, #15552 ) ;
#17371 = CARTESIAN_POINT ( 'NONE',  ( 31.66250999073069750, -5.675955295111851484, -3.283357778048667797 ) ) ;
#17372 = ORIENTED_EDGE ( 'NONE', *, *, #13595, .T. ) ;
#17373 = CARTESIAN_POINT ( 'NONE',  ( 25.72395281601508898, -4.937620572523835349, -7.939653947423662039 ) ) ;
#17374 = PLANE ( 'NONE',  #1498 ) ;
#17375 = CARTESIAN_POINT ( 'NONE',  ( -5.499998817156067865, -20.49639288455253450, 6.000000000000000000 ) ) ;
#17376 = CARTESIAN_POINT ( 'NONE',  ( 0.000000000000000000, 0.000000000000000000, 1.102182119232618281E-16 ) ) ;
#17377 = CARTESIAN_POINT ( 'NONE',  ( 30.01512236704901682, -6.601339762873093875, -7.033357778048666908 ) ) ;
#17378 = CARTESIAN_POINT ( 'NONE',  ( 31.53813789838894621, -6.745008222462202774, -5.783357778048668685 ) ) ;
#17379 = VECTOR ( 'NONE', #130, 1000.000000000000114 ) ;
#17380 = EDGE_LOOP ( 'NONE', ( #8697, #8136, #10551, #5660 ) ) ;
#17381 = LINE ( 'NONE', #11630, #17337 ) ;
#17382 = CARTESIAN_POINT ( 'NONE',  ( 26.94172295629870462, -6.971623697019761146, -7.033357778048666908 ) ) ;
#17383 = CARTESIAN_POINT ( 'NONE',  ( -1.144235203016674918, -3.958177651039095135, -0.09382832055446259367 ) ) ;
#17384 = VERTEX_POINT ( 'NONE', #16035 ) ;
#17385 = CARTESIAN_POINT ( 'NONE',  ( 33.95908713831676096, -3.945449517755638791, -3.283357778048664688 ) ) ;
#17386 = CIRCLE ( 'NONE', #12426, 14.00000000000000178 ) ;
#17387 = PRODUCT_DEFINITION_SHAPE ( 'NONE', 'NONE',  #14229 ) ;
#17388 = FACE_OUTER_BOUND ( 'NONE', #1610, .T. ) ;
#17389 = CARTESIAN_POINT ( 'NONE',  ( 25.75668387115780078, -2.745663783273349257, -5.690028976746116740 ) ) ;
#17390 = CARTESIAN_POINT ( 'NONE',  ( 32.07220196432898263, -5.426722983814484813, -3.627061608673668225 ) ) ;
#17391 = CARTESIAN_POINT ( 'NONE',  ( 30.08145424927873535, -6.930706697444451336, 5.783357778048664244 ) ) ;
#17392 = EDGE_CURVE ( 'NONE', #6854, #16186, #11978, .T. ) ;
#17393 = CIRCLE ( 'NONE', #15622, 2.000000000000001776 ) ;
#17394 = CARTESIAN_POINT ( 'NONE',  ( 28.72797218747911074, -6.756415940301135237, -4.533357778048668685 ) ) ;
#17395 = CARTESIAN_POINT ( 'NONE',  ( -0.6920835326022560796, -4.454600218803894229, -3.297382984111586257 ) ) ;
#17396 = ITEM_DEFINED_TRANSFORMATION ( 'NONE', 'NONE', #6240,  #3575 ) ;
#17397 = DIRECTION ( 'NONE',  ( 0.000000000000000000, 0.000000000000000000, 1.000000000000000000 ) ) ;
#17398 = DIRECTION ( 'NONE',  ( -1.224646799147353207E-16, 1.000000000000000000, 0.000000000000000000 ) ) ;
#17399 = CARTESIAN_POINT ( 'NONE',  ( 31.54230778485832332, -2.355712103769039611, -4.705209693361160461 ) ) ;
#17400 = DIRECTION ( 'NONE',  ( 1.000000000000000000, 0.000000000000000000, 0.000000000000000000 ) ) ;
#17401 = CARTESIAN_POINT ( 'NONE',  ( 1.296864337298335788E-21, -1.182044466681725685E-21, -6.899999999999998579 ) ) ;
#17402 = CARTESIAN_POINT ( 'NONE',  ( 33.64386668575551198, -3.983427357176565486, 3.283357778048664244 ) ) ;
#17403 = VECTOR ( 'NONE', #10480, 1000.000000000000227 ) ;
#17404 = EDGE_LOOP ( 'NONE', ( #7343, #11870, #3015 ) ) ;
#17405 = LINE ( 'NONE', #10784, #9047 ) ;
#17406 = EDGE_CURVE ( 'NONE', #2327, #3955, #11563, .T. ) ;
#17407 = ORIENTED_EDGE ( 'NONE', *, *, #14606, .F. ) ;
#17408 = CARTESIAN_POINT ( 'NONE',  ( 32.08959525433819238, -2.916745304588811649, 3.627061608673666893 ) ) ;
#17409 = CARTESIAN_POINT ( 'NONE',  ( -4.101948962585906244, -2.368261337751083939, -3.381124513963624345 ) ) ;
#17410 = B_SPLINE_CURVE_WITH_KNOTS ( 'NONE', 3,
 ( #3603, #6221, #11920, #9293, #14586, #6126, #9203, #2337, #8941, #13384, #6495, #17592, #2067, #16206, #17311, #870, #6402, #15837, #3771, #696, #7496, #13019, #605, #4761, #4848, #10377, #15931, #2162, #780, #7679, #11829, #9373, #17678, #10806, #16380, #5371, #17851, #1313, #15180, #10721, #10890, #5199, #16459, #2582 ),
 .UNSPECIFIED., .F., .F.,
 ( 4, 2, 2, 2, 2, 2, 2, 2, 2, 2, 2, 2, 2, 2, 2, 2, 2, 2, 2, 2, 2, 4 ),
 ( 0.000000000000000000, 0.001235571410315390150, 0.001853357115473088478, 0.002471142820630786805, 0.003706714230946187797, 0.004324499936103893064, 0.004942285641261598764, 0.006177857051577013633, 0.007413428461892427636, 0.008031214167050130734, 0.008648999872207834699, 0.009884571282523253039, 0.01112014269283866964, 0.01235571410315408972, 0.01297349980831179542, 0.01359128551346949765, 0.01482685692378490731, 0.01606242833410031698, 0.01668021403925802268, 0.01729799974441572491, 0.01853357115473113284, 0.01976914256504654077 ),
 .UNSPECIFIED. ) ;
#17411 = ORIENTED_EDGE ( 'NONE', *, *, #5600, .F. ) ;
#17412 = CARTESIAN_POINT ( 'NONE',  ( 26.31175009776946538, -7.352777558617343168, -6.181997573440047411 ) ) ;
#17413 = ORIENTED_EDGE ( 'NONE', *, *, #14153, .F. ) ;
#17414 = CARTESIAN_POINT ( 'NONE',  ( 26.31137250323187260, -7.349643480353759806, -6.203850694058635540 ) ) ;
#17415 = CARTESIAN_POINT ( 'NONE',  ( 33.43363050022580296, -2.127845067243429256, -4.705209693361160461 ) ) ;
#17416 = EDGE_CURVE ( 'NONE', #8021, #1670, #11561, .T. ) ;
#17417 = CARTESIAN_POINT ( 'NONE',  ( 32.02836186724004364, -4.178063784105134459, -7.939653947423662039 ) ) ;
#17418 = CARTESIAN_POINT ( 'NONE',  ( 31.37049041475757605, -6.775403295959669947, 5.113484796970852564 ) ) ;
#17419 = CARTESIAN_POINT ( 'NONE',  ( 31.68992120585416217, -1.700760206360153015, -5.783357778048664244 ) ) ;
#17420 = CARTESIAN_POINT ( 'NONE',  ( 28.14933959732260149, -3.391468297350501260, -7.939653947423660263 ) ) ;
#17421 = AXIS2_PLACEMENT_3D ( 'NONE', #17560, #8073, #16510 ) ;
#17422 = CARTESIAN_POINT ( 'NONE',  ( 31.34233605952372415, -6.778795339760710803, -5.783357778048663356 ) ) ;
#17423 = CARTESIAN_POINT ( 'NONE',  ( 31.84257795004536007, -2.746633492292519296, -3.283357778048662023 ) ) ;
#17424 = CARTESIAN_POINT ( 'NONE',  ( 32.46178999037268653, -4.125844254797621957, 3.283357778048664244 ) ) ;
#17425 = ORIENTED_EDGE ( 'NONE', *, *, #6293, .F. ) ;
#17426 = CIRCLE ( 'NONE', #15068, 5.000000000000000000 ) ;
#17427 = ORIENTED_EDGE ( 'NONE', *, *, #6917, .T. ) ;
#17428 = CIRCLE ( 'NONE', #13624, 2.000000000000001776 ) ;
#17429 = VERTEX_POINT ( 'NONE', #3607 ) ;
#17430 = EDGE_CURVE ( 'NONE', #548, #2553, #6353, .T. ) ;
#17431 = ORIENTED_EDGE ( 'NONE', *, *, #7966, .T. ) ;
#17432 = CARTESIAN_POINT ( 'NONE',  ( 23.02601376483258022, 3.965314980223224151, 0.000000000000000000 ) ) ;
#17433 = CARTESIAN_POINT ( 'NONE',  ( 32.50119254608192421, -4.121097024973739309, 7.939653947423662039 ) ) ;
#17434 = ORIENTED_EDGE ( 'NONE', *, *, #1433, .F. ) ;
#17435 = CARTESIAN_POINT ( 'NONE',  ( -1.499999999999999112, 5.809475019311125976, -3.000000000000000000 ) ) ;
#17436 = AXIS2_PLACEMENT_3D ( 'NONE', #2914, #16618, #5710 ) ;
#17437 = CARTESIAN_POINT ( 'NONE',  ( 33.12669930479518854, -6.563814807098823145, 6.453230759126467042 ) ) ;
#17438 = CARTESIAN_POINT ( 'NONE',  ( -17.59998316743469715, -19.37170218437266200, -15.90983619775817459 ) ) ;
#17439 = CARTESIAN_POINT ( 'NONE',  ( 29.54591158530375239, -2.596238420101622868, -6.861505862736158257 ) ) ;
#17440 = CARTESIAN_POINT ( 'NONE',  ( -7.511572993685817836E-16, -4.618802153517020059, -3.133295621305386636 ) ) ;
#17441 = CARTESIAN_POINT ( 'NONE',  ( 35.74085044863416982, -18.73429073671341172, -11.27079897466147251 ) ) ;
#17442 = CARTESIAN_POINT ( 'NONE',  ( 31.64365984991007252, -1.316785610144591390, -5.783357778048658027 ) ) ;
#17443 = LINE ( 'NONE', #6526, #11039 ) ;
#17444 = CARTESIAN_POINT ( 'NONE',  ( 17.08564552898659272, -14.18688536295006664, 15.98696333172761719 ) ) ;
#17445 = AXIS2_PLACEMENT_3D ( 'NONE', #15526, #10069, #16994 ) ;
#17446 = EDGE_CURVE ( 'NONE', #6903, #12118, #2071, .T. ) ;
#17447 = CARTESIAN_POINT ( 'NONE',  ( 28.24571643650507369, -4.633797857156355171, -7.939653947423662039 ) ) ;
#17448 = CARTESIAN_POINT ( 'NONE',  ( 31.56875459193803124, -6.114348982704044921, -4.705209693361169343 ) ) ;
#17449 = ORIENTED_EDGE ( 'NONE', *, *, #12039, .T. ) ;
#17450 = DIRECTION ( 'NONE',  ( -0.1196152422706611984, 0.9928203230275510771, 0.000000000000000000 ) ) ;
#17451 = VECTOR ( 'NONE', #2449, 1000.000000000000000 ) ;
#17452 = CARTESIAN_POINT ( 'NONE',  ( 26.14503574297738098, -5.691300421908874085, 3.283357778048664688 ) ) ;
#17453 = EDGE_CURVE ( 'NONE', #15678, #15612, #14668, .T. ) ;
#17454 = ORIENTED_EDGE ( 'NONE', *, *, #12170, .F. ) ;
#17455 = CARTESIAN_POINT ( 'NONE',  ( 26.00347982711925710, -2.723222710571018279, 4.533357778048667797 ) ) ;
#17456 = EDGE_CURVE ( 'NONE', #17637, #12969, #206, .T. ) ;
#17457 = CIRCLE ( 'NONE', #1207, 2.749999999999988454 ) ;
#17458 = CARTESIAN_POINT ( 'NONE',  ( 33.38562051666750818, -5.268481986227246949, -7.939653947423662927 ) ) ;
#17459 = VERTEX_POINT ( 'NONE', #3412 ) ;
#17460 = CARTESIAN_POINT ( 'NONE',  ( 29.16815758536418102, -2.004582921727632971, -5.783357778048664244 ) ) ;
#17461 = CARTESIAN_POINT ( 'NONE',  ( 27.85662501549087366, -2.162596695673018043, -5.113484796970851676 ) ) ;
#17462 = EDGE_LOOP ( 'NONE', ( #6285, #16663, #13017, #15973 ) ) ;
#17463 = CIRCLE ( 'NONE', #3830, 10.50000000000000000 ) ;
#17464 = CYLINDRICAL_SURFACE ( 'NONE', #17758, 2.500000000000001776 ) ;
#17465 = CARTESIAN_POINT ( 'NONE',  ( 31.94023320572814484, -7.096308717197083560, -5.783357778048669573 ) ) ;
#17466 = ADVANCED_FACE ( 'NONE', ( #1977 ), #7499, .F. ) ;
#17467 = CARTESIAN_POINT ( 'NONE',  ( 28.97253418081003673, -5.800171738120336151, -7.939653947423664704 ) ) ;
#17468 = AXIS2_PLACEMENT_3D ( 'NONE', #10659, #13416, #14778 ) ;
#17469 = CARTESIAN_POINT ( 'NONE',  ( 26.06962060539356330, -5.343074812781621219, -3.590724507760069795 ) ) ;
#17470 = CARTESIAN_POINT ( 'NONE',  ( 7.374038404635931521, -5.989453865500120600, -2.000000000000000000 ) ) ;
#17471 = CARTESIAN_POINT ( 'NONE',  ( 0.5449245075115098924, 4.304189842417216028, -3.016622336523194114 ) ) ;
#17472 = ORIENTED_EDGE ( 'NONE', *, *, #13518, .F. ) ;
#17473 = CARTESIAN_POINT ( 'NONE',  ( 28.09001152836989235, -6.106370808549102414, -8.283357778048662468 ) ) ;
#17474 = CARTESIAN_POINT ( 'NONE',  ( 30.62726312072365431, -1.838986382273682718, -5.783357778048658915 ) ) ;
#17475 = EDGE_CURVE ( 'NONE', #3702, #15383, #5115, .T. ) ;
#17476 = EDGE_LOOP ( 'NONE', ( #6554, #6223, #1993, #12570 ) ) ;
#17477 = EDGE_CURVE ( 'NONE', #15522, #10591, #5374, .T. ) ;
#17478 = B_SPLINE_CURVE_WITH_KNOTS ( 'NONE', 3,
 ( #17105, #12911, #15455, #8837 ),
 .UNSPECIFIED., .F., .F.,
 ( 4, 4 ),
 ( 0.004328141481285538092, 0.004974662558709086295 ),
 .UNSPECIFIED. ) ;
#17479 = PRODUCT_RELATED_PRODUCT_CATEGORY ( 'part', '', ( #6352 ) ) ;
#17480 = VERTEX_POINT ( 'NONE', #8020 ) ;
#17481 = CARTESIAN_POINT ( 'NONE',  ( 5.000000000000000888, 0.000000000000000000, 0.000000000000000000 ) ) ;
#17482 = CARTESIAN_POINT ( 'NONE',  ( 30.48043329534786849, -5.818372192732907067, -3.283357778048667797 ) ) ;
#17483 = DIRECTION ( 'NONE',  ( -0.000000000000000000, -0.000000000000000000, 1.000000000000000000 ) ) ;
#17484 = VERTEX_POINT ( 'NONE', #17681 ) ;
#17485 = CARTESIAN_POINT ( 'NONE',  ( 21.42601376483257880, 2.765314980223224417, 6.000000000000000000 ) ) ;
#17486 = FACE_OUTER_BOUND ( 'NONE', #13378, .T. ) ;
#17487 = CARTESIAN_POINT ( 'NONE',  ( 33.56062403295735663, -2.739515387291123982, -3.627061608673662008 ) ) ;
#17488 = DIRECTION ( 'NONE',  ( 0.000000000000000000, 1.000000000000000000, -4.661026453772598353E-17 ) ) ;
#17489 = AXIS2_PLACEMENT_3D ( 'NONE', #9209, #13210, #702 ) ;
#17490 = MANIFOLD_SOLID_BREP ( 'Sweep1', #13900 ) ;
#17491 = VECTOR ( 'NONE', #2387, 1000.000000000000114 ) ;
#17492 = ADVANCED_FACE ( 'NONE', ( #17768 ), #9376, .F. ) ;
#17493 = CARTESIAN_POINT ( 'NONE',  ( 27.23057351405260818, -1.848475362037681480, -5.783357778048658027 ) ) ;
#17494 = CARTESIAN_POINT ( 'NONE',  ( 39.55500000000002103, 0.000000000000000000, 0.000000000000000000 ) ) ;
#17495 = EDGE_CURVE ( 'NONE', #2702, #8269, #12286, .T. ) ;
#17496 = CARTESIAN_POINT ( 'NONE',  ( 27.19802975513453092, -2.241944418315925613, 5.783357778048667797 ) ) ;
#17497 = CARTESIAN_POINT ( 'NONE',  ( 26.01652455409633902, -4.902371455920926380, 5.783357778048663356 ) ) ;
#17498 = ORIENTED_EDGE ( 'NONE', *, *, #16801, .F. ) ;
#17499 = CARTESIAN_POINT ( 'NONE',  ( 31.43723430067123914, -2.368371383576012956, -6.861505862736158257 ) ) ;
#17500 = DIRECTION ( 'NONE',  ( -5.026720092345836698E-22, 4.581671729415424240E-22, -1.000000000000000000 ) ) ;
#17501 = CARTESIAN_POINT ( 'NONE',  ( 27.11643206945770146, -20.93856092459426677, -13.95341982493238753 ) ) ;
#17502 = AXIS2_PLACEMENT_3D ( 'NONE', #7329, #12846, #6028 ) ;
#17503 = CARTESIAN_POINT ( 'NONE',  ( 27.23882169172318513, -6.009049854935478052, 3.627061608673662896 ) ) ;
#17504 = VERTEX_POINT ( 'NONE', #10558 ) ;
#17505 =( BOUNDED_CURVE ( )  B_SPLINE_CURVE ( 2, ( #181, #12602, #5604, #8607, #11120, #1729, #16779, #7259, #16689 ),
 .UNSPECIFIED., .F., .T. ) 
 B_SPLINE_CURVE_WITH_KNOTS ( ( 3, 2, 2, 2, 3 ),
 ( 0.2115384615384615641, 0.2179487179487179516, 0.2307692307692307820, 0.2435897435897435848, 0.2500000000000000000 ),
 .UNSPECIFIED. ) 
 CURVE ( )  GEOMETRIC_REPRESENTATION_ITEM ( )  RATIONAL_B_SPLINE_CURVE ( ( 0.9330127018922194093, 0.9330127018922196314, 1.000000000000000000, 0.8660254037844387076, 1.000000000000000000, 0.8660254037844387076, 1.000000000000000000, 0.9330127018922191873, 0.9330127018922194093 ) ) 
 REPRESENTATION_ITEM ( '' )  );
#17506 = STYLED_ITEM ( 'NONE', ( #8559 ), #17610 ) ;
#17507 = ORIENTED_EDGE ( 'NONE', *, *, #11187, .F. ) ;
#17508 = AXIS2_PLACEMENT_3D ( 'NONE', #4924, #2230, #7744 ) ;
#17509 = ORIENTED_EDGE ( 'NONE', *, *, #12262, .T. ) ;
#17510 = CARTESIAN_POINT ( 'NONE',  ( 30.15443244188179150, -1.895953141405084086, 5.783357778048668685 ) ) ;
#17511 = DIRECTION ( 'NONE',  ( -1.224646799147353207E-16, 1.000000000000000000, 0.000000000000000000 ) ) ;
#17512 = ORIENTED_EDGE ( 'NONE', *, *, #9645, .T. ) ;
#17513 = FILL_AREA_STYLE ('',( #5202 ) ) ;
#17514 = PLANE ( 'NONE',  #9264 ) ;
#17516 = AXIS2_PLACEMENT_3D ( 'NONE', #15969, #7707, #11773 ) ;
#17515 = CARTESIAN_POINT ( 'NONE',  ( 41.60261161686052134, -0.5064767720214741198, -5.783357778048662468 ) ) ;
#17517 = CARTESIAN_POINT ( 'NONE',  ( 32.30426898124760982, -6.025734024055190652, -6.861505862736167138 ) ) ;
#17518 = CARTESIAN_POINT ( 'NONE',  ( 30.88125018618674744, -3.062327022369072171, -3.627061608673662896 ) ) ;
#17519 = CYLINDRICAL_SURFACE ( 'NONE', #6032, 2.749999999999992006 ) ;
#17520 = CIRCLE ( 'NONE', #15746, 5.000000000000000000 ) ;
#17521 = LINE ( 'NONE', #9136, #17403 ) ;
#17522 =( NAMED_UNIT ( * ) SI_UNIT ( $, .STERADIAN. ) SOLID_ANGLE_UNIT ( ) );
#17523 = CARTESIAN_POINT ( 'NONE',  ( 26.86653773853314320, -2.919050055179571945, -6.861505862736159145 ) ) ;
#17524 = EDGE_CURVE ( 'NONE', #8513, #3428, #5291, .T. ) ;
#17525 =( BOUNDED_CURVE ( )  B_SPLINE_CURVE ( 3, ( #7302, #12909, #3211, #9012 ),
 .UNSPECIFIED., .F., .T. ) 
 B_SPLINE_CURVE_WITH_KNOTS ( ( 4, 4 ),
 ( 1.514099494053832595, 1.567750514535811712 ),
 .UNSPECIFIED. ) 
 CURVE ( )  GEOMETRIC_REPRESENTATION_ITEM ( )  RATIONAL_B_SPLINE_CURVE ( ( 1.000000000000000000, 0.9997601450507493936, 0.9997601450507493936, 1.000000000000000000 ) ) 
 REPRESENTATION_ITEM ( '' )  );
#17526 = DIRECTION ( 'NONE',  ( 0.000000000000000000, 0.000000000000000000, -1.000000000000000000 ) ) ;
#17527 = CARTESIAN_POINT ( 'NONE',  ( -36.27615609941022257, -23.17738945083361557, -0.000000000000000000 ) ) ;
#17528 = LINE ( 'NONE', #4863, #16522 ) ;
#17529 = CARTESIAN_POINT ( 'NONE',  ( 26.97551107961034944, -7.694459687869362519, 5.783357778048657138 ) ) ;
#17530 = EDGE_LOOP ( 'NONE', ( #17805, #7227, #7376, #8894 ) ) ;
#17531 = EDGE_CURVE ( 'NONE', #6798, #14747, #9462, .T. ) ;
#17532 = ORIENTED_EDGE ( 'NONE', *, *, #5330, .T. ) ;
#17533 = CARTESIAN_POINT ( 'NONE',  ( 26.01652455409633902, -4.902371455920928156, -5.783357778048663356 ) ) ;
#17534 = VECTOR ( 'NONE', #17225, 1000.000000000000000 ) ;
#17535 = CARTESIAN_POINT ( 'NONE',  ( 31.97277696464621854, -6.702839660918840536, -5.783357778048663356 ) ) ;
#17536 = ORIENTED_EDGE ( 'NONE', *, *, #12545, .F. ) ;
#17537 = DIRECTION ( 'NONE',  ( 0.1196152422706609902, -0.9928203230275510771, 0.000000000000000000 ) ) ;
#17538 = CARTESIAN_POINT ( 'NONE',  ( 29.78250536075762867, -6.329556739422670830, -6.861505862736167138 ) ) ;
#17539 = CARTESIAN_POINT ( 'NONE',  ( 30.49166216014303643, -4.363205751385915931, -8.283357778048662468 ) ) ;
#17540 = B_SPLINE_CURVE_WITH_KNOTS ( 'NONE', 3,
 ( #4987, #3644, #13159, #10515, #10327, #5073, #15882, #6077 ),
 .UNSPECIFIED., .F., .F.,
 ( 4, 2, 2, 4 ),
 ( 0.005725059856848630467, 0.006314084072593618806, 0.006903108288338607144, 0.008081156719828584689 ),
 .UNSPECIFIED. ) ;
#17541 = CARTESIAN_POINT ( 'NONE',  ( 1.500000000000000000, 11.00000000000000000, -2.000000000000000000 ) ) ;
#17542 = CARTESIAN_POINT ( 'NONE',  ( 26.56758885001203652, -2.317900097157796324, -5.783357778048670461 ) ) ;
#17543 = CARTESIAN_POINT ( 'NONE',  ( 23.43390247958827288, -9.970148115950962620, 14.83177094038517652 ) ) ;
#17544 = EDGE_CURVE ( 'NONE', #2945, #8113, #16307, .T. ) ;
#17545 = VECTOR ( 'NONE', #17746, 1000.000000000000114 ) ;
#17546 = CARTESIAN_POINT ( 'NONE',  ( 31.45915434921569798, -2.992700983430681028, -7.939653947423660263 ) ) ;
#17547 = CARTESIAN_POINT ( 'NONE',  ( 33.30663696749426350, -1.516174747195734085, -5.783357778048658915 ) ) ;
#17548 = VERTEX_POINT ( 'NONE', #1234 ) ;
#17549 = FACE_OUTER_BOUND ( 'NONE', #11221, .T. ) ;
#17550 = CARTESIAN_POINT ( 'NONE',  ( 26.75784435724945709, -6.993777436889428323, 7.033357778048657138 ) ) ;
#17551 = EDGE_CURVE ( 'NONE', #4281, #11111, #7027, .T. ) ;
#17552 = PRODUCT_DEFINITION_SHAPE ( 'NONE', 'NONE',  #14992 ) ;
#17553 = VERTEX_POINT ( 'NONE', #970 ) ;
#17554 = DIRECTION ( 'NONE',  ( 0.9928203230275512992, 0.1196152422706610180, 4.006172263299093133E-17 ) ) ;
#17555 = CARTESIAN_POINT ( 'NONE',  ( 33.17547354829333983, -5.293800545841212291, -3.627061608673667781 ) ) ;
#17556 = ORIENTED_EDGE ( 'NONE', *, *, #12700, .F. ) ;
#17557 = EDGE_CURVE ( 'NONE', #2500, #12046, #17627, .T. ) ;
#17558 = LINE ( 'NONE', #8166, #9859 ) ;
#17559 = CARTESIAN_POINT ( 'NONE',  ( 26.16909369068367752, -6.168712907020689862, -7.925803108758818105 ) ) ;
#17560 = CARTESIAN_POINT ( 'NONE',  ( -31.74999999999995737, 0.000000000000000000, 0.000000000000000000 ) ) ;
#17561 = CARTESIAN_POINT ( 'NONE',  ( 29.74110826630371207, -2.999819088432076786, -8.283357778048660691 ) ) ;
#17562 = CARTESIAN_POINT ( 'NONE',  ( 33.06225340847440464, -6.234220648470727433, -4.533357778048668685 ) ) ;
#17563 = ORIENTED_EDGE ( 'NONE', *, *, #11046, .F. ) ;
#17564 = CARTESIAN_POINT ( 'NONE',  ( 32.75517961154501023, -5.344437665069116328, -7.939653947423664704 ) ) ;
#17565 = CARTESIAN_POINT ( 'NONE',  ( 26.31176419598820360, -7.352894575460818594, -6.182016197336221985 ) ) ;
#17566 = DIRECTION ( 'NONE',  ( 1.000000000000000000, 0.000000000000000000, -0.000000000000000000 ) ) ;
#17567 = CARTESIAN_POINT ( 'NONE',  ( 13.34918303132433692, 14.15390528054681596, -16.46429318744779025 ) ) ;
#17568 = CARTESIAN_POINT ( 'NONE',  ( 29.86122125502053848, -4.439161430227785310, -8.283357778048662468 ) ) ;
#17569 = CARTESIAN_POINT ( 'NONE',  ( 32.54050588463559990, -2.235448945602741766, -6.861505862736159145 ) ) ;
#17570 = EDGE_CURVE ( 'NONE', #2553, #17048, #13478, .T. ) ;
#17571 = ORIENTED_EDGE ( 'NONE', *, *, #13855, .F. ) ;
#17572 = DIRECTION ( 'NONE',  ( -0.5661261679878573094, 0.8243186046180107640, 0.000000000000000000 ) ) ;
#17573 = CARTESIAN_POINT ( 'NONE',  ( 26.61823960964035507, -2.311797680896151341, -6.453230759126464378 ) ) ;
#17574 = VERTEX_POINT ( 'NONE', #5825 ) ;
#17575 = DIRECTION ( 'NONE',  ( 0.000000000000000000, 0.000000000000000000, 1.000000000000000000 ) ) ;
#17576 = DIRECTION ( 'NONE',  ( 1.000000000000000000, 1.224646799147353207E-16, 0.000000000000000000 ) ) ;
#17577 = DIRECTION ( 'NONE',  ( -5.026720092345836698E-22, 4.581671729415424240E-22, -1.000000000000000000 ) ) ;
#17578 = DIRECTION ( 'NONE',  ( -0.000000000000000000, 1.000000000000000000, -0.000000000000000000 ) ) ;
#17579 = ORIENTED_EDGE ( 'NONE', *, *, #17358, .F. ) ;
#17580 = CARTESIAN_POINT ( 'NONE',  ( 30.06013935859953534, -5.869009311960810216, -8.283357778048662468 ) ) ;
#17581 = CARTESIAN_POINT ( 'NONE',  ( 20.00000000000000000, 7.999999999999996447, 12.00000000000000000 ) ) ;
#17582 = CARTESIAN_POINT ( 'NONE',  ( -3.248936832696171617, -20.49508120620799900, 78.00000000000000000 ) ) ;
#17583 = DIRECTION ( 'NONE',  ( -0.000000000000000000, -1.000000000000000000, 3.469446951953614189E-16 ) ) ;
#17584 = VERTEX_POINT ( 'NONE', #5555 ) ;
#17585 = CARTESIAN_POINT ( 'NONE',  ( 28.28502977505876359, -2.748149777785362957, -6.861505862736158257 ) ) ;
#17586 = CARTESIAN_POINT ( 'NONE',  ( 33.14902674121363901, -1.535163666906202318, -5.783357778048658027 ) ) ;
#17587 = CARTESIAN_POINT ( 'NONE',  ( 27.69265652961275848, -20.36619546179435503, -13.80192434669152490 ) ) ;
#17588 = CARTESIAN_POINT ( 'NONE',  ( 27.04606801335823718, -3.524390735323772006, 3.627061608673666893 ) ) ;
#17589 = ORIENTED_EDGE ( 'NONE', *, *, #15442, .F. ) ;
#17590 = ADVANCED_FACE ( 'NONE', ( #9809 ), #8374, .T. ) ;
#17591 = CARTESIAN_POINT ( 'NONE',  ( 30.39102621733566423, -5.629271460726126719, 3.627061608673662896 ) ) ;
#17592 = CARTESIAN_POINT ( 'NONE',  ( -27.68235608956435811, -12.07326681422359194, 13.80428259828453896 ) ) ;
#17593 = DIRECTION ( 'NONE',  ( 0.000000000000000000, 0.000000000000000000, -1.000000000000000000 ) ) ;
#17594 = EDGE_CURVE ( 'NONE', #2265, #14461, #11351, .T. ) ;
#17595 = ORIENTED_EDGE ( 'NONE', *, *, #4191, .T. ) ;
#17596 = CARTESIAN_POINT ( 'NONE',  ( 33.13353876934985465, -5.498725377814142057, -8.283357778048664244 ) ) ;
#17597 = LINE ( 'NONE', #5116, #7541 ) ;
#17598 = ORIENTED_EDGE ( 'NONE', *, *, #17456, .T. ) ;
#17599 = CARTESIAN_POINT ( 'NONE',  ( 1.746467850512308208E-21, -1.591841644184202181E-21, -6.005572809000082835 ) ) ;
#17600 = FACE_OUTER_BOUND ( 'NONE', #167, .T. ) ;
#17601 =( BOUNDED_CURVE ( )  B_SPLINE_CURVE ( 2, ( #379, #1734, #12878, #10316, #8889, #14423, #14058, #7532, #7264 ),
 .UNSPECIFIED., .F., .T. ) 
 B_SPLINE_CURVE_WITH_KNOTS ( ( 3, 2, 2, 2, 3 ),
 ( 0.7115384615384615641, 0.7179487179487179516, 0.7307692307692307265, 0.7435897435897436125, 0.7500000000000000000 ),
 .UNSPECIFIED. ) 
 CURVE ( )  GEOMETRIC_REPRESENTATION_ITEM ( )  RATIONAL_B_SPLINE_CURVE ( ( 0.9330127018922194093, 0.9330127018922194093, 1.000000000000000000, 0.8660254037844387076, 1.000000000000000000, 0.8660254037844387076, 1.000000000000000000, 0.9330127018922194093, 0.9330127018922194093 ) ) 
 REPRESENTATION_ITEM ( '' )  );
#17602 = CARTESIAN_POINT ( 'NONE',  ( 31.39792096211754924, -4.254019462947003838, -7.939653947423662039 ) ) ;
#17603 = CARTESIAN_POINT ( 'NONE',  ( 4.197393957002304887, 7.725818140447171444E-14, -3.203767560748932208 ) ) ;
#17604 = DIRECTION ( 'NONE',  ( -1.000000000000000000, -0.000000000000000000, -0.000000000000000000 ) ) ;
#17605 = CARTESIAN_POINT ( 'NONE',  ( 26.34117031759772942, -2.982346454214467535, 6.861505862736165362 ) ) ;
#17606 =( BOUNDED_CURVE ( )  B_SPLINE_CURVE ( 2, ( #16900, #17642, #5250, #12416, #17818, #4181, #1363, #5161, #2467 ),
 .UNSPECIFIED., .F., .T. ) 
 B_SPLINE_CURVE_WITH_KNOTS ( ( 3, 2, 2, 2, 3 ),
 ( 0.8269230769230769829, 0.8333333333333333703, 0.8461538461538461453, 0.8589743589743589203, 0.8653846153846154188 ),
 .UNSPECIFIED. ) 
 CURVE ( )  GEOMETRIC_REPRESENTATION_ITEM ( )  RATIONAL_B_SPLINE_CURVE ( ( 0.9330127018922192983, 0.9330127018922198534, 1.000000000000000000, 0.8660254037844387076, 1.000000000000000000, 0.8660254037844387076, 1.000000000000000000, 0.9330127018922187432, 0.9330127018922192983 ) ) 
 REPRESENTATION_ITEM ( '' )  );
#17607 = DIRECTION ( 'NONE',  ( -0.5000000000000014433, -0.8660254037844378194, 0.000000000000000000 ) ) ;
#17608 = DIRECTION ( 'NONE',  ( -0.000000000000000000, -0.000000000000000000, -1.000000000000000000 ) ) ;
#17609 = DIRECTION ( 'NONE',  ( 0.000000000000000000, 0.000000000000000000, -1.000000000000000000 ) ) ;
#17610 = MANIFOLD_SOLID_BREP ( 'Cavity1', #12740 ) ;
#17611 = CARTESIAN_POINT ( 'NONE',  ( 27.26436163736424945, -2.571311352887278190, 4.533357778048667797 ) ) ;
#17612 = VERTEX_POINT ( 'NONE', #4478 ) ;
#17613 = ORIENTED_EDGE ( 'NONE', *, *, #12370, .F. ) ;
#17614 = EDGE_LOOP ( 'NONE', ( #11944, #15929, #13495 ) ) ;
#17615 = CARTESIAN_POINT ( 'NONE',  ( 31.91459173804834748, -5.445711903524953712, 7.939653947423658487 ) ) ;
#17616 = CARTESIAN_POINT ( 'NONE',  ( 30.78487334700428235, -1.819997462563214263, 5.783357778048668685 ) ) ;
#17617 = AXIS2_PLACEMENT_3D ( 'NONE', #15157, #11048, #1559 ) ;
#17618 = EDGE_LOOP ( 'NONE', ( #14578, #4382 ) ) ;
#17619 = CARTESIAN_POINT ( 'NONE',  ( 31.12210306526553083, -4.287250072544045665, -8.283357778048662468 ) ) ;
#17620 = EDGE_CURVE ( 'NONE', #17612, #6838, #15735, .T. ) ;
#17621 = CARTESIAN_POINT ( 'NONE',  ( 29.94002636988270538, -4.429666970165102136, -8.283357778048662468 ) ) ;
#17622 = DIRECTION ( 'NONE',  ( 0.000000000000000000, 0.000000000000000000, -1.000000000000000000 ) ) ;
#17623 = CARTESIAN_POINT ( 'NONE',  ( 30.80679339554874119, -2.444327062417882779, -6.861505862736158257 ) ) ;
#17624 = CARTESIAN_POINT ( 'NONE',  ( 29.37220822929407760, -7.016156836349003001, 5.783357778048657138 ) ) ;
#17625 = DIRECTION ( 'NONE',  ( -0.000000000000000000, -0.000000000000000000, -1.000000000000000000 ) ) ;
#17626 = LINE ( 'NONE', #16065, #16014 ) ;
#17627 =( BOUNDED_CURVE ( )  B_SPLINE_CURVE ( 2, ( #14752, #12013, #13293, #873, #11924, #17596, #10635, #3774, #2422 ),
 .UNSPECIFIED., .F., .T. ) 
 B_SPLINE_CURVE_WITH_KNOTS ( ( 3, 2, 2, 2, 3 ),
 ( 0.09615384615384617306, 0.1025641025641025605, 0.1153846153846153910, 0.1282051282051281937, 0.1346153846153846367 ),
 .UNSPECIFIED. ) 
 CURVE ( )  GEOMETRIC_REPRESENTATION_ITEM ( )  RATIONAL_B_SPLINE_CURVE ( ( 0.9330127018922194093, 0.9330127018922196314, 1.000000000000000000, 0.8660254037844387076, 1.000000000000000000, 0.8660254037844387076, 1.000000000000000000, 0.9330127018922190762, 0.9330127018922194093 ) ) 
 REPRESENTATION_ITEM ( '' )  );
#17628 = CARTESIAN_POINT ( 'NONE',  ( 26.41562710823574278, -3.600346414165641828, -7.939653947423660263 ) ) ;
#17629 = CARTESIAN_POINT ( 'NONE',  ( 18.46842688268906230, -11.90892979872008084, 15.77307170257308933 ) ) ;
#17630 = EDGE_CURVE ( 'NONE', #11134, #3677, #15616, .T. ) ;
#17631 = CARTESIAN_POINT ( 'NONE',  ( 30.82871344409320713, -3.068656662272551738, -7.939653947423660263 ) ) ;
#17632 = CARTESIAN_POINT ( 'NONE',  ( 30.93831368681553684, -6.190304661545915188, -4.705209693361169343 ) ) ;
#17633 = ORIENTED_EDGE ( 'NONE', *, *, #5099, .T. ) ;
#17634 = DIRECTION ( 'NONE',  ( -0.1196152422706611984, 0.9928203230275510771, 0.000000000000000000 ) ) ;
#17635 = CARTESIAN_POINT ( 'NONE',  ( -8.249999999999923617, 6.495190528383386841, -3.000000000000002665 ) ) ;
#17636 = AXIS2_PLACEMENT_3D ( 'NONE', #7275, #1652, #9966 ) ;
#17637 = VERTEX_POINT ( 'NONE', #4126 ) ;
#17638 = CARTESIAN_POINT ( 'NONE',  ( 31.51169109130924184, -2.986371343527201905, 7.939653947423662927 ) ) ;
#17639 = CARTESIAN_POINT ( 'NONE',  ( 29.64681518302145946, -6.972875258987813574, -5.783357778048668685 ) ) ;
#17640 = EDGE_CURVE ( 'NONE', #6789, #1845, #16907, .T. ) ;
#17641 = DIRECTION ( 'NONE',  ( 0.8660254037844363761, -0.5000000000000038858, 0.000000000000000000 ) ) ;
#17642 = CARTESIAN_POINT ( 'NONE',  ( 26.90109536843240789, -7.313877135454839973, -5.113484796970856117 ) ) ;
#17643 = DIRECTION ( 'NONE',  ( -0.7866107318554605987, 0.6174492339697383869, 8.659560562354860135E-17 ) ) ;
#17644 = CARTESIAN_POINT ( 'NONE',  ( 2.725758460532925920, -3.045084772582431043, -2.920601398289156769 ) ) ;
#17645 = CARTESIAN_POINT ( 'NONE',  ( 31.75254397038802878, -4.211294393702175398, -8.283357778048662468 ) ) ;
#17646 = EDGE_CURVE ( 'NONE', #15348, #5172, #10882, .T. ) ;
#17647 = CONICAL_SURFACE ( 'NONE', #2541, 2.540000000000001368, 0.7853981633974502774 ) ;
#17648 = CARTESIAN_POINT ( 'NONE',  ( 8.409399735147211686E-16, 4.618802153517009401, -3.133295621305383083 ) ) ;
#17649 = CARTESIAN_POINT ( 'NONE',  ( 26.23123039439649062, -6.684454722870800225, -4.255767710538254534 ) ) ;
#17650 = CARTESIAN_POINT ( 'NONE',  ( 0.000000000000000000, 0.000000000000000000, -4.000000000000000000 ) ) ;
#17651 = CARTESIAN_POINT ( 'NONE',  ( 26.75784435724945709, -6.993777436889428323, -4.533357778048668685 ) ) ;
#17652 = CARTESIAN_POINT ( 'NONE',  ( 30.45225960443380231, -4.367952981209816343, -3.627061608673664672 ) ) ;
#17653 = VECTOR ( 'NONE', #4006, 1000.000000000000114 ) ;
#17654 = ORIENTED_EDGE ( 'NONE', *, *, #5987, .F. ) ;
#17655 = AXIS2_PLACEMENT_3D ( 'NONE', #270, #5875, #538 ) ;
#17656 = ORIENTED_EDGE ( 'NONE', *, *, #9180, .T. ) ;
#17657 = DIRECTION ( 'NONE',  ( 0.000000000000000000, 0.000000000000000000, 1.000000000000000000 ) ) ;
#17658 = CARTESIAN_POINT ( 'NONE',  ( -28.41103551745680633, -13.06362195986656616, -13.60745115249024728 ) ) ;
#17659 = AXIS2_PLACEMENT_3D ( 'NONE', #5026, #8012, #13551 ) ;
#17660 = ORIENTED_EDGE ( 'NONE', *, *, #8457, .F. ) ;
#17661 = DIRECTION ( 'NONE',  ( -0.000000000000000000, -0.000000000000000000, 1.000000000000000000 ) ) ;
#17662 = DIRECTION ( 'NONE',  ( 1.000000000000000000, 0.000000000000000000, -0.000000000000000000 ) ) ;
#17663 = CARTESIAN_POINT ( 'NONE',  ( 32.29974222271236073, -2.891426744974864071, -3.627061608673662008 ) ) ;
#17664 = CARTESIAN_POINT ( 'NONE',  ( 3.999999999999999112, 2.309401076758498927, -3.204271511726786148 ) ) ;
#17665 = CARTESIAN_POINT ( 'NONE',  ( 26.60013260893011378, -1.924431040879551746, -5.783357778048658027 ) ) ;
#17666 = CARTESIAN_POINT ( 'NONE',  ( 25.71748644841968456, -2.420320648352046078, -5.783357778048663356 ) ) ;
#17667 = FACE_OUTER_BOUND ( 'NONE', #2196, .T. ) ;
#17668 = CARTESIAN_POINT ( 'NONE',  ( 25.89690931182567724, -3.909551132893385184, 5.783357778048662468 ) ) ;
#17669 = CARTESIAN_POINT ( 'NONE',  ( 26.01127209431523113, -6.877383572197488526, -7.035051132944705188 ) ) ;
#17670 = CIRCLE ( 'NONE', #10932, 9.500000000000001776 ) ;
#17671 = EDGE_CURVE ( 'NONE', #13726, #757, #6004, .T. ) ;
#17672 = FACE_BOUND ( 'NONE', #9708, .T. ) ;
#17673 = CARTESIAN_POINT ( 'NONE',  ( 31.87265695910486230, -5.650636735497883478, 3.283357778048663800 ) ) ;
#17674 = VERTEX_POINT ( 'NONE', #17289 ) ;
#17675 = CIRCLE ( 'NONE', #6350, 4.000000000000000000 ) ;
#17676 = AXIS2_PLACEMENT_3D ( 'NONE', #55, #7132, #1784 ) ;
#17677 = CARTESIAN_POINT ( 'NONE',  ( 28.30694982360322953, -3.372479377640031473, 3.627061608673666893 ) ) ;
#17678 = CARTESIAN_POINT ( 'NONE',  ( -18.90926271784950075, -11.47470670281267857, 15.70082023719634989 ) ) ;
#17679 = LINE ( 'NONE', #12365, #13577 ) ;
#17680 = VERTEX_POINT ( 'NONE', #4744 ) ;
#17681 = CARTESIAN_POINT ( 'NONE',  ( 38.68147913031998542, -1.341155523753224887, -9.283357778048653586 ) ) ;
#17682 = AXIS2_PLACEMENT_3D ( 'NONE', #1897, #4424, #524 ) ;
#17683 = CARTESIAN_POINT ( 'NONE',  ( 26.01652455409633902, -4.902371455920926380, -5.783357778048663356 ) ) ;
#17684 = EDGE_LOOP ( 'NONE', ( #8019, #16886, #13286, #9627, #15722, #16782, #170, #2356, #3723, #14520, #10183, #14134, #17512, #754, #8594 ) ) ;
#17685 = CARTESIAN_POINT ( 'NONE',  ( 26.31176419598820360, -7.352894575460818594, -6.182016197336221985 ) ) ;
#17686 = CARTESIAN_POINT ( 'NONE',  ( 29.80442540930208750, -6.953886339277345563, -5.783357778048669573 ) ) ;
#17687 = CARTESIAN_POINT ( 'NONE',  ( 30.74004950963507810, -6.851358974801540214, -6.453230759126470595 ) ) ;
#17688 = CARTESIAN_POINT ( 'NONE',  ( -23.00000000000000000, -16.21813761408365195, -18.00000000000000355 ) ) ;
#17689 = CARTESIAN_POINT ( 'NONE',  ( 26.98483462626008134, -4.785709214840094816, 3.627061608673664228 ) ) ;
#17690 = AXIS2_PLACEMENT_3D ( 'NONE', #15254, #16911, #16813 ) ;
#17691 = ADVANCED_FACE ( 'NONE', ( #8653 ), #4700, .F. ) ;
#17692 = CYLINDRICAL_SURFACE ( 'NONE', #11639, 2.500000000000001776 ) ;
#17693 = CARTESIAN_POINT ( 'NONE',  ( 31.31418170428987224, -6.782187383561751659, -5.113484796970860558 ) ) ;
#17694 = CARTESIAN_POINT ( 'NONE',  ( 32.69811611091622439, -2.216460025892273311, 4.705209693361168455 ) ) ;
#17695 = CARTESIAN_POINT ( 'NONE',  ( 27.32822876973539294, -6.198150586942257512, 8.283357778048658915 ) ) ;
#17696 = VECTOR ( 'NONE', #12413, 1000.000000000000000 ) ;
#17697 = ORIENTED_EDGE ( 'NONE', *, *, #12076, .F. ) ;
#17698 = VERTEX_POINT ( 'NONE', #7397 ) ;
#17699 = ORIENTED_EDGE ( 'NONE', *, *, #13921, .F. ) ;
#17700 = CARTESIAN_POINT ( 'NONE',  ( 33.42946061375642586, -6.517141185936593750, 5.783357778048658027 ) ) ;
#17701 = LINE ( 'NONE', #5223, #10196 ) ;
#17702 = EDGE_CURVE ( 'NONE', #15783, #8066, #762, .T. ) ;
#17703 = CARTESIAN_POINT ( 'NONE',  ( 30.93831368681553684, -6.190304661545915188, 6.861505862736157368 ) ) ;
#17704 = ORIENTED_EDGE ( 'NONE', *, *, #3137, .F. ) ;
#17705 =( BOUNDED_CURVE ( )  B_SPLINE_CURVE ( 2, ( #4584, #1889, #6027, #12845, #435, #150, #12928, #5939, #12654 ),
 .UNSPECIFIED., .F., .T. ) 
 B_SPLINE_CURVE_WITH_KNOTS ( ( 3, 2, 2, 2, 3 ),
 ( 0.1346153846153846367, 0.1410256410256410242, 0.1538461538461538547, 0.1666666666666666574, 0.1730769230769231004 ),
 .UNSPECIFIED. ) 
 CURVE ( )  GEOMETRIC_REPRESENTATION_ITEM ( )  RATIONAL_B_SPLINE_CURVE ( ( 0.9330127018922194093, 0.9330127018922196314, 1.000000000000000000, 0.8660254037844387076, 1.000000000000000000, 0.8660254037844387076, 1.000000000000000000, 0.9330127018922190762, 0.9330127018922194093 ) ) 
 REPRESENTATION_ITEM ( '' )  );
#17706 = DIRECTION ( 'NONE',  ( -0.9237280213470682178, -0.3830490080632377170, 0.000000000000000000 ) ) ;
#17707 = CARTESIAN_POINT ( 'NONE',  ( 32.26971135134834867, -1.630906943779925955, 6.453230759126469707 ) ) ;
#17708 = CARTESIAN_POINT ( 'NONE',  ( 29.84999239022537409, -5.894327871574777333, -3.283357778048667797 ) ) ;
#17709 = CARTESIAN_POINT ( 'NONE',  ( 29.67743187657054449, -6.342216019229654833, -4.705209693361169343 ) ) ;
#17710 = CARTESIAN_POINT ( 'NONE',  ( 33.76207435632690590, -3.969185667289998332, 7.939653947423662039 ) ) ;
#17711 = APPLICATION_CONTEXT ( 'automotive_design' ) ;
#17712 = CARTESIAN_POINT ( 'NONE',  ( -2.000000000000002220, 3.464101615137751278, 0.000000000000000000 ) ) ;
#17713 = CARTESIAN_POINT ( 'NONE',  ( 31.95146207396702565, -5.641142275435199416, 3.283357778048663356 ) ) ;
#17714 = DIRECTION ( 'NONE',  ( 0.1113444980252557837, 0.9937818688019538493, 0.000000000000000000 ) ) ;
#17715 = LINE ( 'NONE', #3537, #973 ) ;
#17716 = EDGE_CURVE ( 'NONE', #4517, #11475, #77, .T. ) ;
#17717 = CARTESIAN_POINT ( 'NONE',  ( 30.60986983071443390, -4.348964061499348333, -3.627061608673664672 ) ) ;
#17718 = VECTOR ( 'NONE', #6752, 1000.000000000000227 ) ;
#17719 = CARTESIAN_POINT ( 'NONE',  ( 33.13163345120441505, -4.045141346131868154, -3.627061608673664672 ) ) ;
#17720 = ORIENTED_EDGE ( 'NONE', *, *, #5277, .T. ) ;
#17721 = CYLINDRICAL_SURFACE ( 'NONE', #15304, 2.499999999999999112 ) ;
#17722 = DIRECTION ( 'NONE',  ( -0.000000000000000000, -1.000000000000000000, -0.000000000000000000 ) ) ;
#17723 = VERTEX_POINT ( 'NONE', #7475 ) ;
#17724 = CLOSED_SHELL ( 'NONE', ( #935, #2564, #16166, #5969, #4132, #4045, #13818, #1930, #12101, #7035, #2427, #6780, #6875, #12445, #14907, #15471, #14160, #15459, #9541, #4313, #795, #11321, #16064, #13285, #10399, #13111, #1748, #7311, #4063, #5729, #2670, #734, #14942, #4690, #8578, #889, #6946, #8723, #12873 ) ) ;
#17725 = VERTEX_POINT ( 'NONE', #11533 ) ;
#17726 = CARTESIAN_POINT ( 'NONE',  ( 30.86385689617753059, -5.572304701594727128, 3.627061608673662896 ) ) ;
#17727 = CARTESIAN_POINT ( 'NONE',  ( 27.51889869220010354, -3.467423976192371526, -7.939653947423660263 ) ) ;
#17728 =( BOUNDED_CURVE ( )  B_SPLINE_CURVE ( 2, ( #11130, #14149, #2818, #1561, #8346, #8439, #14067, #13974, #9776 ),
 .UNSPECIFIED., .F., .T. ) 
 B_SPLINE_CURVE_WITH_KNOTS ( ( 3, 2, 2, 2, 3 ),
 ( 0.3653846153846154188, 0.3717948717948718063, 0.3846153846153846367, 0.3974358974358974117, 0.4038461538461538547 ),
 .UNSPECIFIED. ) 
 CURVE ( )  GEOMETRIC_REPRESENTATION_ITEM ( )  RATIONAL_B_SPLINE_CURVE ( ( 0.9330127018922194093, 0.9330127018922196314, 1.000000000000000000, 0.8660254037844387076, 1.000000000000000000, 0.8660254037844387076, 1.000000000000000000, 0.9330127018922190762, 0.9330127018922194093 ) ) 
 REPRESENTATION_ITEM ( '' )  );
#17729 = DIRECTION ( 'NONE',  ( 0.9928203230275512992, 0.1196152422706610041, 9.614813431917824012E-17 ) ) ;
#17730 = CARTESIAN_POINT ( 'NONE',  ( 28.45891156537951971, -2.090033060632186412, -5.783357778048670461 ) ) ;
#17731 = DIRECTION ( 'NONE',  ( -0.1196152422706610735, 0.9928203230275511881, 0.000000000000000000 ) ) ;
#17732 = AXIS2_PLACEMENT_3D ( 'NONE', #17494, #5020, #15916 ) ;
#17733 = CARTESIAN_POINT ( 'NONE',  ( 32.93004296264515318, -25.68697430340742471, -12.29384923381407546 ) ) ;
#17734 = CARTESIAN_POINT ( 'NONE',  ( 29.95125523467787687, -2.974500528818130096, -3.283357778048662023 ) ) ;
#17735 = AXIS2_PLACEMENT_3D ( 'NONE', #16690, #11405, #15415 ) ;
#17736 = STYLED_ITEM ( 'NONE', ( #17885 ), #11756 ) ;
#17737 = DIRECTION ( 'NONE',  ( 0.000000000000000000, 0.000000000000000000, 1.000000000000000000 ) ) ;
#17738 = DIRECTION ( 'NONE',  ( 1.000000000000000000, 5.329070518200751394E-15, 0.000000000000000000 ) ) ;
#17739 = CARTESIAN_POINT ( 'NONE',  ( 30.61177514885986639, -5.802548093181622235, -8.283357778048664244 ) ) ;
#17740 = CARTESIAN_POINT ( 'NONE',  ( 33.78529456515154550, -6.484467084455914687, -5.783357778048663356 ) ) ;
#17741 =( BOUNDED_CURVE ( )  B_SPLINE_CURVE ( 2, ( #12585, #9494, #10846, #17966, #15035, #12399, #1270, #1176, #8319 ),
 .UNSPECIFIED., .F., .T. ) 
 B_SPLINE_CURVE_WITH_KNOTS ( ( 3, 2, 2, 2, 3 ),
 ( 0.8269230769230769829, 0.8333333333333333703, 0.8461538461538461453, 0.8589743589743589203, 0.8653846153846154188 ),
 .UNSPECIFIED. ) 
 CURVE ( )  GEOMETRIC_REPRESENTATION_ITEM ( )  RATIONAL_B_SPLINE_CURVE ( ( 0.9330127018922192983, 0.9330127018922198534, 1.000000000000000000, 0.8660254037844387076, 1.000000000000000000, 0.8660254037844387076, 1.000000000000000000, 0.9330127018922187432, 0.9330127018922192983 ) ) 
 REPRESENTATION_ITEM ( '' )  );
#17742 = CARTESIAN_POINT ( 'NONE',  ( -12.70000000000000284, 0.000000000000000000, 0.000000000000000000 ) ) ;
#17743 = EDGE_CURVE ( 'NONE', #17723, #627, #3481, .T. ) ;
#17744 = CARTESIAN_POINT ( 'NONE',  ( 33.17094678975809074, -2.159493266760871499, -6.861505862736159145 ) ) ;
#17745 = AXIS2_PLACEMENT_3D ( 'NONE', #6457, #5160, #16164 ) ;
#17746 = DIRECTION ( 'NONE',  ( 0.1196152422706609625, -0.9928203230275510771, 4.694733121053620740E-17 ) ) ;
#17747 = VECTOR ( 'NONE', #8839, 1000.000000000000000 ) ;
#17748 = DIRECTION ( 'NONE',  ( 1.000000000000000000, 0.000000000000000000, 0.000000000000000000 ) ) ;
#17749 = VERTEX_POINT ( 'NONE', #17385 ) ;
#17750 = CARTESIAN_POINT ( 'NONE',  ( 30.40841950734487753, -3.119293781500474427, -3.627061608673662008 ) ) ;
#17751 = CARTESIAN_POINT ( 'NONE',  ( -19.43845002722867221, 2.988003976273734263, 6.000000000000000000 ) ) ;
#17752 = CIRCLE ( 'NONE', #3834, 2.041999999999999815 ) ;
#17753 = CARTESIAN_POINT ( 'NONE',  ( 33.17094678975809074, -2.159493266760871499, -6.861505862736159145 ) ) ;
#17754 = CARTESIAN_POINT ( 'NONE',  ( 4.101954839143060916, -2.368264730582942956, -3.381130640444271584 ) ) ;
#17755 = VECTOR ( 'NONE', #3777, 999.9999999999998863 ) ;
#17756 = DIRECTION ( 'NONE',  ( 0.000000000000000000, 0.000000000000000000, -1.000000000000000000 ) ) ;
#17757 = CARTESIAN_POINT ( 'NONE',  ( 28.49970350196817392, -5.857138497251738407, -7.939653947423664704 ) ) ;
#17758 = AXIS2_PLACEMENT_3D ( 'NONE', #6182, #17273, #9171 ) ;
#17759 = EDGE_CURVE ( 'NONE', #7588, #3845, #674, .T. ) ;
#17760 = CARTESIAN_POINT ( 'NONE',  ( 29.08710323061924896, -17.65086537115787380, -13.41876697690134179 ) ) ;
#17761 = CARTESIAN_POINT ( 'NONE',  ( 31.30979230060565044, -7.172264396038955603, 5.783357778048657138 ) ) ;
#17762 = ORIENTED_EDGE ( 'NONE', *, *, #16280, .T. ) ;
#17763 = EDGE_CURVE ( 'NONE', #2226, #6664, #2125, .T. ) ;
#17764 = CARTESIAN_POINT ( 'NONE',  ( 30.91186687973582536, -2.431667782610909434, 6.861505862736166250 ) ) ;
#17765 = CARTESIAN_POINT ( 'NONE',  ( -23.00000000000000000, -16.21813761408365195, 13.00000000000000355 ) ) ;
#17766 = CARTESIAN_POINT ( 'NONE',  ( 28.74176732417158320, -7.092112515190875044, 5.783357778048669573 ) ) ;
#17767 = ORIENTED_EDGE ( 'NONE', *, *, #15431, .F. ) ;
#17768 = FACE_OUTER_BOUND ( 'NONE', #13178, .T. ) ;
#17769 = AXIS2_PLACEMENT_3D ( 'NONE', #552, #17607, #5045 ) ;
#17770 = ORIENTED_EDGE ( 'NONE', *, *, #3769, .T. ) ;
#17771 = AXIS2_PLACEMENT_3D ( 'NONE', #2526, #8054, #6786 ) ;
#17772 = DIRECTION ( 'NONE',  ( 0.9928203230275512992, 0.1196152422706614898, -0.000000000000000000 ) ) ;
#17773 = EDGE_CURVE ( 'NONE', #15658, #16745, #6731, .T. ) ;
#17774 = ORIENTED_EDGE ( 'NONE', *, *, #7991, .F. ) ;
#17775 = ORIENTED_EDGE ( 'NONE', *, *, #15110, .F. ) ;
#17776 = DIRECTION ( 'NONE',  ( 0.1196152422706621143, 0.9928203230275509661, 0.000000000000000000 ) ) ;
#17777 = CARTESIAN_POINT ( 'NONE',  ( 29.13014440709066832, -5.781182818409868140, -7.939653947423664704 ) ) ;
#17778 = FACE_OUTER_BOUND ( 'NONE', #3498, .T. ) ;
#17779 = FACE_OUTER_BOUND ( 'NONE', #12366, .T. ) ;
#17780 = CARTESIAN_POINT ( 'NONE',  ( 25.83772294520678159, -3.669972453104032084, 7.939653947423664704 ) ) ;
#17781 = CARTESIAN_POINT ( 'NONE',  ( 28.86293393808771057, -2.678523738846987357, 6.861505862736165362 ) ) ;
#17782 = CARTESIAN_POINT ( 'NONE',  ( 32.97895737133300287, -1.545456804875372958, 6.453230759126471483 ) ) ;
#17783 = DIRECTION ( 'NONE',  ( 0.9928203230275512992, 0.1196152422706610180, 4.006172263299093133E-17 ) ) ;
#17784 = DIRECTION ( 'NONE',  ( -0.000000000000000000, -0.000000000000000000, 1.000000000000000000 ) ) ;
#17785 = VECTOR ( 'NONE', #6019, 1000.000000000000000 ) ;
#17786 = CARTESIAN_POINT ( 'NONE',  ( 29.39961944441754227, -3.040961747597316300, 8.283357778048664244 ) ) ;
#17787 = ORIENTED_EDGE ( 'NONE', *, *, #11835, .T. ) ;
#17788 = ORIENTED_EDGE ( 'NONE', *, *, #14348, .T. ) ;
#17789 = ORIENTED_EDGE ( 'NONE', *, *, #12255, .T. ) ;
#17790 = CARTESIAN_POINT ( 'NONE',  ( 30.88125018618674744, -3.062327022369072171, 7.939653947423664704 ) ) ;
#17791 = AXIS2_PLACEMENT_3D ( 'NONE', #1984, #1626, #15667 ) ;
#17792 = CARTESIAN_POINT ( 'NONE',  ( 25.74999999999999645, -16.21813761408365195, 0.000000000000000000 ) ) ;
#17793 = CARTESIAN_POINT ( 'NONE',  ( 29.14753769709988518, -3.271205139184214072, 7.939653947423662927 ) ) ;
#17794 = DIRECTION ( 'NONE',  ( -0.9928203230275512992, -0.1196152422706610180, -9.614813431917824012E-17 ) ) ;
#17795 = CARTESIAN_POINT ( 'NONE',  ( 33.76207435632690590, -3.969185667289998332, -3.627061608673664672 ) ) ;
#17796 = ADVANCED_FACE ( 'NONE', ( #1868 ), #7659, .F. ) ;
#17797 = CARTESIAN_POINT ( 'NONE',  ( -4.000000000000000000, -2.309401076758510918, -0.5000000000000000000 ) ) ;
#17798 = CARTESIAN_POINT ( 'NONE',  ( 26.39370705969127684, -2.976016814310973313, -6.861505862736158257 ) ) ;
#17799 = CARTESIAN_POINT ( 'NONE',  ( 29.71979337562451207, -1.938121702948446323, 5.783357778048662468 ) ) ;
#17800 = CARTESIAN_POINT ( 'NONE',  ( 10.40000000000000036, 1.273632671113247276E-15, 0.000000000000000000 ) ) ;
#17801 = DIRECTION ( 'NONE',  ( -0.5000000000000008882, 0.8660254037844382635, 0.000000000000000000 ) ) ;
#17802 = CARTESIAN_POINT ( 'NONE',  ( 29.04511322243489602, -14.57839366656647506, -13.43065377816253481 ) ) ;
#17803 = DIRECTION ( 'NONE',  ( -0.000000000000000000, -0.000000000000000000, -1.000000000000000000 ) ) ;
#17804 = SURFACE_SIDE_STYLE ('',( #9411 ) ) ;
#17805 = ORIENTED_EDGE ( 'NONE', *, *, #9380, .F. ) ;
#17806 = CARTESIAN_POINT ( 'NONE',  ( 31.43723430067123914, -2.368371383576012956, -6.861505862736158257 ) ) ;
#17807 = CARTESIAN_POINT ( 'NONE',  ( 29.97942892559193950, -4.424919740341219487, -3.627061608673664672 ) ) ;
#17808 = DIRECTION ( 'NONE',  ( -0.000000000000000000, 0.000000000000000000, -1.000000000000000000 ) ) ;
#17809 = AXIS2_PLACEMENT_3D ( 'NONE', #4974, #17625, #9156 ) ;
#17810 = DIRECTION ( 'NONE',  ( -0.6000000000000000888, -0.7999999999999999334, -0.000000000000000000 ) ) ;
#17811 =( BOUNDED_CURVE ( )  B_SPLINE_CURVE ( 2, ( #13270, #17487, #10618, #16190, #14901, #9274, #3664, #3484, #9189, #7662, #14816, #5015, #2406, #10702, #11812, #7928, #13461, #13544, #1120, #6644, #6557, #12077, #2144, #12172, #11904, #17663, #4830, #765, #15911, #9015, #14566, #9107, #16010, #13187, #3585, #17390, #4923, #10451, #14647, #16710, #15170, #11141, #15248, #1387, #9700, #10876, #2829, #4283, #16446, #6732, #5275, #6910, #1574, #9788, #12349, #16369, #3932, #4108, #15341, #2919, #7107, #17750, #5448, #4200, #8270, #13719, #2751, #9530, #26, #9444, #2661, #10792, #14982, #17917, #13802, #4014, #8357, #13888, #6824, #8453, #12439, #11062, #5537, #1477, #2569, #8096, #8193, #10968, #7007, #13631, #16529, #1301, #1217, #12270, #17839, #9616, #16622, #5357, #12532, #116, #5623, #13990, #15075, #5809, #12981, #396, #4727, #1939, #15438, #11425, #9973, #10250, #15800, #14076, #11329, #3021, #1852, #3374, #8543, #5986, #8907, #16905, #4636, #8821, #1755, #14442, #7380, #12706, #2025, #16807, #11614, #10162, #1661, #12621, #7196, #12802, #15711, #7457, #298, #5902, #565, #16990, #4545, #4461, #11512, #3290, #6085, #15523, #17082 ),
 .UNSPECIFIED., .F., .T. ) 
 B_SPLINE_CURVE_WITH_KNOTS ( ( 3, 2, 2, 2, 2, 2, 2, 2, 2, 2, 2, 2, 2, 2, 2, 2, 2, 2, 2, 2, 2, 2, 2, 2, 2, 2, 2, 2, 2, 2, 2, 2, 2, 2, 2, 2, 2, 2, 2, 2, 2, 2, 2, 2, 2, 2, 2, 2, 2, 2, 2, 2, 2, 2, 2, 2, 2, 2, 2, 2, 2, 2, 2, 2, 2, 2, 2, 2, 2, 2, 2, 2, 2, 2, 3 ),
 ( 0.000000000000000000, 0.01322951878407230102, 0.02645903756814460203, 0.03968855635221691519, 0.05291807513628920406, 0.06614759392036151375, 0.07937711270443383038, 0.09260663148850611925, 0.1058361502725784081, 0.1190656690566507248, 0.1322951878407230275, 0.1455247066247953303, 0.1587542254088676608, 0.1719837441929399358, 0.1852132629770122385, 0.1984427817610845690, 0.2116723005451568163, 0.2249018193292291468, 0.2381313381133014495, 0.2513608568973737523, 0.2645903756814460550, 0.2778198944655183578, 0.2910494132495906605, 0.3042789320336629633, 0.3175084508177353215, 0.3307379696018076243, 0.3439674883858798715, 0.3571970071699521743, 0.3704265259540244770, 0.3836560447380968353, 0.3968855635221691380, 0.4101150823062413853, 0.4233446010903136325, 0.4365741198743859908, 0.4498036386584582935, 0.4630331574425305963, 0.4762626762266028990, 0.4894921950106752018, 0.5027217137947475045, 0.5159512325788198073, 0.5291807513628921100, 0.5424102701469644128, 0.5556397889310367155, 0.5688693077151090183, 0.5820988264991813210, 0.5953283452832536238, 0.6085578640673259265, 0.6217873828513982293, 0.6350169016354706431, 0.6482464204195428348, 0.6614759392036152486, 0.6747054579876874403, 0.6879349767717597430, 0.7011644955558321568, 0.7143940143399043485, 0.7276235331239767623, 0.7408530519080489540, 0.7540825706921212568, 0.7673120894761936706, 0.7805416082602658623, 0.7937711270443382761, 0.8070006458284105788, 0.8202301646124827705, 0.8334596833965551843, 0.8466892021806272650, 0.8599187209646996788, 0.8731482397487719815, 0.8863777585328441733, 0.8996072773169165870, 0.9128367961009887788, 0.9260663148850611925, 0.9392958336691334953, 0.9525253524532057980, 0.9657548712372781008, 0.9750618896629086318 ),
 .UNSPECIFIED. ) 
 CURVE ( )  GEOMETRIC_REPRESENTATION_ITEM ( )  RATIONAL_B_SPLINE_CURVE ( ( 1.000000000000000000, 0.8660254037844387076, 1.000000000000000000, 0.8660254037844387076, 1.000000000000000000, 0.8660254037844387076, 1.000000000000000000, 0.8660254037844387076, 1.000000000000000000, 0.8660254037844387076, 1.000000000000000000, 0.8660254037844387076, 1.000000000000000000, 0.8660254037844387076, 1.000000000000000000, 0.8660254037844387076, 1.000000000000000000, 0.8660254037844387076, 1.000000000000000000, 0.8660254037844387076, 1.000000000000000000, 0.8660254037844387076, 1.000000000000000000, 0.8660254037844387076, 1.000000000000000000, 0.8660254037844387076, 1.000000000000000000, 0.8660254037844387076, 1.000000000000000000, 0.8660254037844387076, 1.000000000000000000, 0.8660254037844387076, 1.000000000000000000, 0.8660254037844387076, 1.000000000000000000, 0.8660254037844387076, 1.000000000000000000, 0.8660254037844387076, 1.000000000000000000, 0.8660254037844387076, 1.000000000000000000, 0.8660254037844387076, 1.000000000000000000, 0.8660254037844387076, 1.000000000000000000, 0.8660254037844387076, 1.000000000000000000, 0.8660254037844387076, 1.000000000000000000, 0.8660254037844387076, 1.000000000000000000, 0.8660254037844387076, 1.000000000000000000, 0.8660254037844387076, 1.000000000000000000, 0.8660254037844387076, 1.000000000000000000, 0.8660254037844387076, 1.000000000000000000, 0.8660254037844387076, 1.000000000000000000, 0.8660254037844387076, 1.000000000000000000, 0.8660254037844387076, 1.000000000000000000, 0.8660254037844387076, 1.000000000000000000, 0.8660254037844387076, 1.000000000000000000, 0.8660254037844387076, 1.000000000000000000, 0.8660254037844387076, 1.000000000000000000, 0.8660254037844387076, 1.000000000000000000, 0.8660254037844387076, 1.000000000000000000, 0.8660254037844387076, 1.000000000000000000, 0.8660254037844387076, 1.000000000000000000, 0.8660254037844387076, 1.000000000000000000, 0.8660254037844387076, 1.000000000000000000, 0.8660254037844387076, 1.000000000000000000, 0.8660254037844387076, 1.000000000000000000, 0.8660254037844387076, 1.000000000000000000, 0.8660254037844387076, 1.000000000000000000, 0.8660254037844387076, 1.000000000000000000, 0.8660254037844387076, 1.000000000000000000, 0.8660254037844387076, 1.000000000000000000, 0.8660254037844387076, 1.000000000000000000, 0.8660254037844387076, 1.000000000000000000, 0.8660254037844387076, 1.000000000000000000, 0.8660254037844387076, 1.000000000000000000, 0.8660254037844387076, 1.000000000000000000, 0.8660254037844387076, 1.000000000000000000, 0.8660254037844387076, 1.000000000000000000, 0.8660254037844387076, 1.000000000000000000, 0.8660254037844387076, 1.000000000000000000, 0.8660254037844387076, 1.000000000000000000, 0.8660254037844387076, 1.000000000000000000, 0.8660254037844387076, 1.000000000000000000, 0.8660254037844387076, 1.000000000000000000, 0.8660254037844387076, 1.000000000000000000, 0.8660254037844387076, 1.000000000000000000, 0.8660254037844387076, 1.000000000000000000, 0.8660254037844387076, 1.000000000000000000, 0.8660254037844387076, 1.000000000000000000, 0.8660254037844387076, 1.000000000000000000, 0.8660254037844387076, 1.000000000000000000, 0.8660254037844387076, 1.000000000000000000, 0.8660254037844387076, 1.000000000000000000, 0.8660254037844387076, 1.000000000000000000, 0.8660254037844387076, 1.000000000000000000, 0.9057483453558528019, 0.9441095091726994237 ) ) 
 REPRESENTATION_ITEM ( '' )  );
#17812 = ORIENTED_EDGE ( 'NONE', *, *, #3192, .T. ) ;
#17813 = CARTESIAN_POINT ( 'NONE',  ( 31.91006497951310550, -2.311404624444611589, 4.705209693361167567 ) ) ;
#17814 = CARTESIAN_POINT ( 'NONE',  ( 30.27725608814395386, -6.896919580145944195, -5.783357778048668685 ) ) ;
#17815 = CARTESIAN_POINT ( 'NONE',  ( 29.45101334415624095, -7.006662376286320715, 5.783357778048669573 ) ) ;
#17816 = EDGE_CURVE ( 'NONE', #9808, #15632, #13088, .T. ) ;
#17817 = DIRECTION ( 'NONE',  ( 0.000000000000000000, 0.000000000000000000, 1.000000000000000000 ) ) ;
#17818 = CARTESIAN_POINT ( 'NONE',  ( 26.47260139170898441, -4.847423203795396596, -3.283357778048664688 ) ) ;
#17819 = EDGE_CURVE ( 'NONE', #122, #4537, #17525, .T. ) ;
#17820 = CARTESIAN_POINT ( 'NONE',  ( 28.36392410707646761, -4.619556167269785796, -3.283357778048664688 ) ) ;
#17821 = CARTESIAN_POINT ( 'NONE',  ( -29.25000000000000000, -16.21813761408365195, -13.00000000000000178 ) ) ;
#17822 = CARTESIAN_POINT ( 'NONE',  ( 26.70901672940806648, -4.818939824437135755, -8.283357778048662468 ) ) ;
#17823 = ORIENTED_EDGE ( 'NONE', *, *, #14, .F. ) ;
#17824 = DIRECTION ( 'NONE',  ( -0.000000000000000000, -0.000000000000000000, 1.000000000000000000 ) ) ;
#17825 =( LENGTH_UNIT ( ) NAMED_UNIT ( * ) SI_UNIT ( .MILLI., .METRE. ) );
#17826 = CARTESIAN_POINT ( 'NONE',  ( 1.499999999999999334, -5.809475019311126864, -1.901951201008075243 ) ) ;
#17827 = CARTESIAN_POINT ( 'NONE',  ( 30.35023428074701002, -1.862166024106576057, 5.783357778048662468 ) ) ;
#17828 = CARTESIAN_POINT ( 'NONE',  ( 26.02974819644417792, -2.720057890826728109, -4.533357778048659803 ) ) ;
#17829 = CARTESIAN_POINT ( 'NONE',  ( 28.12741954877813555, -2.767138697495831856, -6.861505862736159145 ) ) ;
#17830 = B_SPLINE_CURVE_WITH_KNOTS ( 'NONE', 3,
 ( #8268, #7921, #6821, #9270, #5271, #12347, #13455, #8091, #17658, #17913, #16527, #5179, #14898, #3929, #13627, #6727, #2916, #4541, #11327, #14074, #16803, #3102, #9882, #13988, #8629, #1474, #4280, #5713, #9971, #1752, #11423, #294, #5806, #5535, #7281, #15435, #12529, #1848, #3189, #12799, #11060, #8355, #15611, #7005 ),
 .UNSPECIFIED., .F., .F.,
 ( 4, 2, 2, 2, 2, 2, 2, 2, 2, 2, 2, 2, 2, 2, 2, 2, 2, 2, 2, 2, 2, 4 ),
 ( 0.000000000000000000, 0.001235571410315390150, 0.001853357115473088478, 0.002471142820630786805, 0.003706714230946187797, 0.004324499936103893064, 0.004942285641261598764, 0.006177857051577013633, 0.007413428461892427636, 0.008031214167050130734, 0.008648999872207834699, 0.009884571282523253039, 0.01112014269283866964, 0.01235571410315408972, 0.01297349980831179542, 0.01359128551346949765, 0.01482685692378490731, 0.01606242833410031698, 0.01668021403925802268, 0.01729799974441572491, 0.01853357115473113284, 0.01976914256504654077 ),
 .UNSPECIFIED. ) ;
#17831 =( BOUNDED_CURVE ( )  B_SPLINE_CURVE ( 2, ( #7479, #9996, #3125, #16828, #323, #3216, #588, #3041, #8658 ),
 .UNSPECIFIED., .F., .T. ) 
 B_SPLINE_CURVE_WITH_KNOTS ( ( 3, 2, 2, 2, 3 ),
 ( 0.4423076923076923461, 0.4487179487179487336, 0.4615384615384615641, 0.4743589743589743390, 0.4807692307692307820 ),
 .UNSPECIFIED. ) 
 CURVE ( )  GEOMETRIC_REPRESENTATION_ITEM ( )  RATIONAL_B_SPLINE_CURVE ( ( 0.9330127018922194093, 0.9330127018922196314, 1.000000000000000000, 0.8660254037844387076, 1.000000000000000000, 0.8660254037844387076, 1.000000000000000000, 0.9330127018922190762, 0.9330127018922194093 ) ) 
 REPRESENTATION_ITEM ( '' )  );
#17832 = VERTEX_POINT ( 'NONE', #6286 ) ;
#17833 = CARTESIAN_POINT ( 'NONE',  ( 42.32030307048450624, -6.463398710186787355, -5.783357778048662468 ) ) ;
#17834 = CARTESIAN_POINT ( 'NONE',  ( 8.632250723006720250, -18.84644399697197770, -16.84735068286506987 ) ) ;
#17835 = ORIENTED_EDGE ( 'NONE', *, *, #17118, .T. ) ;
#17836 = APPLICATION_CONTEXT ( 'automotive_design' ) ;
#17837 = DIRECTION ( 'NONE',  ( -0.000000000000000000, -0.000000000000000000, 1.000000000000000000 ) ) ;
#17838 = ADVANCED_FACE ( 'NONE', ( #492 ), #15908, .F. ) ;
#17839 = CARTESIAN_POINT ( 'NONE',  ( 29.04699097144805364, -6.418171698071525100, -4.705209693361169343 ) ) ;
#17840 = CARTESIAN_POINT ( 'NONE',  ( -6.935828204433864386, -17.68137362934027479, -16.94363565911716663 ) ) ;
#17841 = EDGE_LOOP ( 'NONE', ( #12433, #13510, #11604, #25 ) ) ;
#17842 = CARTESIAN_POINT ( 'NONE',  ( 33.19286683830256379, -2.783822866615540903, -7.939653947423660263 ) ) ;
#17843 = EDGE_CURVE ( 'NONE', #12324, #11446, #17102, .T. ) ;
#17844 = PLANE ( 'NONE',  #10392 ) ;
#17845 = CARTESIAN_POINT ( 'NONE',  ( 4.000000000000000000, -2.511476383524240408, -3.169254053377044134 ) ) ;
#17846 = CARTESIAN_POINT ( 'NONE',  ( 33.95908713831676096, -3.945449517755638791, -3.283357778048664688 ) ) ;
#17847 = ORIENTED_EDGE ( 'NONE', *, *, #528, .F. ) ;
#17848 = DIRECTION ( 'NONE',  ( -0.000000000000000000, -0.000000000000000000, 1.000000000000000000 ) ) ;
#17849 = VERTEX_POINT ( 'NONE', #8835 ) ;
#17850 = CARTESIAN_POINT ( 'NONE',  ( 28.41655006632555569, -6.494127376913395366, 6.861505862736157368 ) ) ;
#17851 = CARTESIAN_POINT ( 'NONE',  ( -17.60362937644963921, -13.05831870693043584, 15.90927928682413928 ) ) ;
#17852 = CARTESIAN_POINT ( 'NONE',  ( 23.00000000000000000, -16.21813761408365195, -13.00000000000000355 ) ) ;
#17853 = ORIENTED_EDGE ( 'NONE', *, *, #5600, .T. ) ;
#17854 = CARTESIAN_POINT ( 'NONE',  ( 0.000000000000000000, 0.000000000000000000, -8.700000000000001066 ) ) ;
#17855 = ORIENTED_EDGE ( 'NONE', *, *, #3681, .T. ) ;
#17856 = CARTESIAN_POINT ( 'NONE',  ( 0.000000000000000000, 0.000000000000000000, 8.700000000000001066 ) ) ;
#17857 = EDGE_CURVE ( 'NONE', #7588, #13928, #16592, .T. ) ;
#17858 = VERTEX_POINT ( 'NONE', #14371 ) ;
#17859 = DIRECTION ( 'NONE',  ( -0.000000000000000000, -0.000000000000000000, 1.000000000000000000 ) ) ;
#17860 = CARTESIAN_POINT ( 'NONE',  ( 28.26310972651430120, -2.123820177930694442, -5.783357778048658027 ) ) ;
#17861 = DIRECTION ( 'NONE',  ( 0.000000000000000000, 0.000000000000000000, 1.000000000000000000 ) ) ;
#17862 = CARTESIAN_POINT ( 'NONE',  ( 1.500000000000000000, 11.00000000000000000, -9.708203932499369415 ) ) ;
#17863 = SURFACE_STYLE_USAGE ( .BOTH. , #10995 ) ;
#17864 = EDGE_CURVE ( 'NONE', #2720, #4427, #3263, .T. ) ;
#17865 = CARTESIAN_POINT ( 'NONE',  ( 30.88577694472199298, -6.196634301449400084, 4.705209693361160461 ) ) ;
#17866 = CARTESIAN_POINT ( 'NONE',  ( 32.95080301609915097, -1.548848848676412260, 5.783357778048663356 ) ) ;
#17867 = DIRECTION ( 'NONE',  ( 1.000000000000000000, 0.000000000000000000, 0.000000000000000000 ) ) ;
#17868 = CARTESIAN_POINT ( 'NONE',  ( 42.20068782821381603, -5.470578387159230616, -5.783357778048662468 ) ) ;
#17869 = ORIENTED_EDGE ( 'NONE', *, *, #1871, .T. ) ;
#17870 = ORIENTED_EDGE ( 'NONE', *, *, #3866, .T. ) ;
#17871 = CARTESIAN_POINT ( 'NONE',  ( 32.14213199643172914, -2.910415664685331638, 7.939653947423664704 ) ) ;
#17872 = DIRECTION ( 'NONE',  ( 1.000000000000000000, 0.000000000000000000, 0.000000000000000000 ) ) ;
#17873 = ORIENTED_EDGE ( 'NONE', *, *, #14468, .T. ) ;
#17874 = CARTESIAN_POINT ( 'NONE',  ( 31.02146712245815507, -5.553315781884258229, 3.627061608673662896 ) ) ;
#17875 = CARTESIAN_POINT ( 'NONE',  ( 30.96820195323705605, -2.125071739898741097, -7.033357778048658027 ) ) ;
#17876 = DIRECTION ( 'NONE',  ( 0.000000000000000000, 0.000000000000000000, 1.000000000000000000 ) ) ;
#17877 = ORIENTED_EDGE ( 'NONE', *, *, #15704, .F. ) ;
#17878 = CARTESIAN_POINT ( 'NONE',  ( 27.57216386142120257, -6.895668018177890879, -7.033357778048666908 ) ) ;
#17879 = CARTESIAN_POINT ( 'NONE',  ( 26.82722439997946395, -4.804698134550569044, -3.627061608673664672 ) ) ;
#17880 = PLANE ( 'NONE',  #7283 ) ;
#17881 = CARTESIAN_POINT ( 'NONE',  ( 31.04700706809921940, -2.115577279836057922, -7.033357778048658027 ) ) ;
#17882 = FACE_OUTER_BOUND ( 'NONE', #15220, .T. ) ;
#17883 = CARTESIAN_POINT ( 'NONE',  ( 18.90607966454165734, -11.47788193099826692, -15.70134094032044736 ) ) ;
#17884 = DIRECTION ( 'NONE',  ( -1.000000000000000000, 0.000000000000000000, 0.000000000000000000 ) ) ;
#17885 = PRESENTATION_STYLE_ASSIGNMENT (( #1271 ) ) ;
#17886 = CARTESIAN_POINT ( 'NONE',  ( 32.91278983782564183, -5.325448745358647429, -7.939653947423664704 ) ) ;
#17887 = CARTESIAN_POINT ( 'NONE',  ( 30.41294626588012306, -6.253601060580800564, -6.861505862736167138 ) ) ;
#17888 = CARTESIAN_POINT ( 'NONE',  ( 25.71748644841968456, -2.420320648352051851, -5.783357778048663356 ) ) ;
#17889 = EDGE_CURVE ( 'NONE', #7654, #15926, #5548, .T. ) ;
#17890 = CARTESIAN_POINT ( 'NONE',  ( -1.500000000000000000, -10.39230484541326405, -3.000000000000002665 ) ) ;
#17891 = ORIENTED_EDGE ( 'NONE', *, *, #3228, .F. ) ;
#17892 = CARTESIAN_POINT ( 'NONE',  ( 31.38469755857769528, -2.374701023479507178, 6.861505862736165362 ) ) ;
#17893 = CARTESIAN_POINT ( 'NONE',  ( 27.10313151398701947, -6.652368374500619908, -6.861505862736166250 ) ) ;
#17894 = CARTESIAN_POINT ( 'NONE',  ( 9.166200962222330162, 3.560057785416366194, -2.333128398347829258 ) ) ;
#17895 = CARTESIAN_POINT ( 'NONE',  ( 28.16881664323204859, -6.096876348486420127, 3.283357778048663356 ) ) ;
#17896 = CARTESIAN_POINT ( 'NONE',  ( 29.64681518302145591, -6.972875258987813574, -5.783357778048668685 ) ) ;
#17897 = DIRECTION ( 'NONE',  ( 0.000000000000000000, 0.000000000000000000, -1.000000000000000000 ) ) ;
#17898 = CYLINDRICAL_SURFACE ( 'NONE', #17421, 4.250000000000000000 ) ;
#17899 = LINE ( 'NONE', #9768, #7003 ) ;
#17900 = CARTESIAN_POINT ( 'NONE',  ( 27.92107091181166467, -2.492190854301117753, -4.533357778048659803 ) ) ;
#17901 = PRODUCT_DEFINITION_FORMATION_WITH_SPECIFIED_SOURCE ( 'ANY', '', #11993, .NOT_KNOWN. ) ;
#17902 = VERTEX_POINT ( 'NONE', #10615 ) ;
#17903 = CARTESIAN_POINT ( 'NONE',  ( 3.333333333333333481, 2.694301256218250007, -3.000726591567081325 ) ) ;
#17904 = CARTESIAN_POINT ( 'NONE',  ( 27.90727577511918867, -2.156494279411373061, -5.783357778048670461 ) ) ;
#17905 = FACE_OUTER_BOUND ( 'NONE', #9906, .T. ) ;
#17906 = DIRECTION ( 'NONE',  ( 1.000000000000000000, 0.000000000000000000, 0.000000000000000000 ) ) ;
#17907 = VERTEX_POINT ( 'NONE', #5013 ) ;
#17908 = CARTESIAN_POINT ( 'NONE',  ( 26.82912971812490355, -6.258282166232842947, -8.283357778048662468 ) ) ;
#17909 = EDGE_CURVE ( 'NONE', #4619, #7917, #4715, .T. ) ;
#17910 = CARTESIAN_POINT ( 'NONE',  ( 28.23249303296521617, -2.754479417688857179, -4.705209693361161349 ) ) ;
#17911 = DIRECTION ( 'NONE',  ( -5.026720092345836698E-22, 4.581671729415424240E-22, -1.000000000000000000 ) ) ;
#17912 = EDGE_LOOP ( 'NONE', ( #5829, #7139 ) ) ;
#17913 = CARTESIAN_POINT ( 'NONE',  ( -28.06754645621478517, -12.55420304724502323, -13.70087619851170757 ) ) ;
#17914 = B_SPLINE_CURVE_WITH_KNOTS ( 'NONE', 3,
 ( #104, #1372, #3008, #5438 ),
 .UNSPECIFIED., .F., .F.,
 ( 4, 4 ),
 ( 2.843119637679310382E-07, 0.001422633878257848579 ),
 .UNSPECIFIED. ) ;
#17915 = ORIENTED_EDGE ( 'NONE', *, *, #11504, .F. ) ;
#17916 = CONICAL_SURFACE ( 'NONE', #5999, 3.999999999999998224, 0.8911886515913775009 ) ;
#17917 = CARTESIAN_POINT ( 'NONE',  ( 29.77797860222238313, -3.195249460342344250, -3.627061608673662008 ) ) ;
#17918 = ORIENTED_EDGE ( 'NONE', *, *, #17306, .F. ) ;
#17919 = DIRECTION ( 'NONE',  ( 0.1113444980252557837, 0.9937818688019538493, 0.000000000000000000 ) ) ;
#17920 = EDGE_LOOP ( 'NONE', ( #17472, #2377, #4770, #2985 ) ) ;
#17921 = CARTESIAN_POINT ( 'NONE',  ( 26.24741491880507027, -3.420740141806666745, -3.283357778048662023 ) ) ;
#17922 = CARTESIAN_POINT ( 'NONE',  ( -15.92260893619738837, -28.39189527176317540, -16.15082599432113142 ) ) ;
#17923 = DIRECTION ( 'NONE',  ( 0.000000000000000000, 0.000000000000000000, -1.000000000000000000 ) ) ;
#17924 = CARTESIAN_POINT ( 'NONE',  ( 27.65458886993626564, -2.824105456627233224, -6.861505862736158257 ) ) ;
#17925 = ORIENTED_EDGE ( 'NONE', *, *, #5679, .F. ) ;
#17926 = CARTESIAN_POINT ( 'NONE',  ( 29.18195272205665347, -2.340279496617377664, -4.533357778048659803 ) ) ;
#17927 = EDGE_LOOP ( 'NONE', ( #11998, #11398, #16142, #732 ) ) ;
#17928 = STYLED_ITEM ( 'NONE', ( #13225 ), #5349 ) ;
#17929 = AXIS2_PLACEMENT_3D ( 'NONE', #5479, #12472, #15196 ) ;
#17930 = CARTESIAN_POINT ( 'NONE',  ( 25.74134610602432360, -2.427642893298174620, 5.783357778048668685 ) ) ;
#17931 = PRESENTATION_STYLE_ASSIGNMENT (( #2764 ) ) ;
#17932 = CARTESIAN_POINT ( 'NONE',  ( 20.27597925817430635, -21.85809165190032743, 15.46244260681514326 ) ) ;
#17933 = ORIENTED_EDGE ( 'NONE', *, *, #12430, .F. ) ;
#17934 = AXIS2_PLACEMENT_3D ( 'NONE', #8717, #15514, #3096 ) ;
#17935 = CARTESIAN_POINT ( 'NONE',  ( 28.08317206381523334, -7.171460237833785278, -5.113484796970862334 ) ) ;
#17936 = CARTESIAN_POINT ( 'NONE',  ( 26.31556265977298992, -7.384422263489805793, 5.783357778048663356 ) ) ;
#17937 = CARTESIAN_POINT ( 'NONE',  ( 30.28142597461332741, -2.507623461452779701, -4.705209693361160461 ) ) ;
#17938 = AXIS2_PLACEMENT_3D ( 'NONE', #5925, #13912, #8479 ) ;
#17939 = DIRECTION ( 'NONE',  ( -1.000000000000000000, 0.000000000000000000, 0.000000000000000000 ) ) ;
#17940 = CARTESIAN_POINT ( 'NONE',  ( 28.72797218747911074, -6.756415940301135237, -4.533357778048668685 ) ) ;
#17941 = DIRECTION ( 'NONE',  ( 0.000000000000000000, 0.000000000000000000, 1.000000000000000000 ) ) ;
#17942 = CARTESIAN_POINT ( 'NONE',  ( 26.45077056032005913, -6.103994453487816330, 3.627061608673662896 ) ) ;
#17943 = CARTESIAN_POINT ( 'NONE',  ( 29.41022140756759029, -3.239556939666760726, 3.627061608673666893 ) ) ;
#17944 = CYLINDRICAL_SURFACE ( 'NONE', #15130, 2.500000000000000888 ) ;
#17945 = DIRECTION ( 'NONE',  ( 0.000000000000000000, 0.000000000000000000, -1.000000000000000000 ) ) ;
#17946 = LINE ( 'NONE', #12473, #6667 ) ;
#17947 = EDGE_CURVE ( 'NONE', #14980, #3522, #4159, .T. ) ;
#17948 = ORIENTED_EDGE ( 'NONE', *, *, #11261, .F. ) ;
#17949 = CIRCLE ( 'NONE', #7514, 6.249999999999998224 ) ;
#17950 = VERTEX_POINT ( 'NONE', #13364 ) ;
#17951 = CARTESIAN_POINT ( 'NONE',  ( 32.12473870642251939, -5.420393343910986594, 3.627061608673662896 ) ) ;
#17952 = DIRECTION ( 'NONE',  ( -0.7681011886108269904, -0.5760758914581204371, 0.2795659695588260107 ) ) ;
#17953 = ORIENTED_EDGE ( 'NONE', *, *, #549, .F. ) ;
#17954 = PRESENTATION_STYLE_ASSIGNMENT (( #10016 ) ) ;
#17955 = EDGE_CURVE ( 'NONE', #9808, #3274, #14377, .T. ) ;
#17956 = CARTESIAN_POINT ( 'NONE',  ( 23.02601376483258022, 3.965314980223224151, 0.000000000000000000 ) ) ;
#17957 = ORIENTED_EDGE ( 'NONE', *, *, #752, .F. ) ;
#17958 = CARTESIAN_POINT ( 'NONE',  ( 27.24868051476284236, -2.235842002054281075, 5.113484796970861446 ) ) ;
#17959 = CARTESIAN_POINT ( 'NONE',  ( 33.59503905791412137, -1.808589744724287129, -4.533357778048659803 ) ) ;
#17960 = CARTESIAN_POINT ( 'NONE',  ( 27.26074174026764751, -6.633379454790151009, -6.861505862736167138 ) ) ;
#17961 = CARTESIAN_POINT ( 'NONE',  ( 29.40036258452792950, -7.012764792547963033, 5.113484796970851676 ) ) ;
#17962 = AXIS2_PLACEMENT_3D ( 'NONE', #14044, #1441, #11110 ) ;
#17963 = CARTESIAN_POINT ( 'NONE',  ( 30.09392748191118017, -6.591845302810410701, -7.033357778048666908 ) ) ;
#17964 = DIRECTION ( 'NONE',  ( -0.1196152422706610735, 0.9928203230275511881, 0.000000000000000000 ) ) ;
#17965 = CARTESIAN_POINT ( 'NONE',  ( 25.01746843935482190, -10.28886876799018246, -14.47312570928799680 ) ) ;
#17966 = CARTESIAN_POINT ( 'NONE',  ( 26.69778786461289855, -6.274106265784127778, 8.283357778048660691 ) ) ;
#17967 = CARTESIAN_POINT ( 'NONE',  ( 25.89388370423996832, -3.884438240559767053, -3.881334880282079514 ) ) ;
#17968 = NEXT_ASSEMBLY_USAGE_OCCURRENCE ( 'NAUO1', ' ', ' ', #16665, #10978, $ ) ;
#17969 = NEXT_ASSEMBLY_USAGE_OCCURRENCE ( 'NAUO2', ' ', ' ', #16665, #1048, $ ) ;
#17970 = NEXT_ASSEMBLY_USAGE_OCCURRENCE ( 'NAUO3', ' ', ' ', #16665, #14229, $ ) ;
#17971 = NEXT_ASSEMBLY_USAGE_OCCURRENCE ( 'NAUO4', ' ', ' ', #16665, #14992, $ ) ;
#17972 = NEXT_ASSEMBLY_USAGE_OCCURRENCE ( 'NAUO5', ' ', ' ', #16665, #15789, $ ) ;
#17973 = NEXT_ASSEMBLY_USAGE_OCCURRENCE ( 'NAUO6', ' ', ' ', #16665, #1048, $ ) ;
#17974 = NEXT_ASSEMBLY_USAGE_OCCURRENCE ( 'NAUO7', ' ', ' ', #16665, #14229, $ ) ;
#17975 = NEXT_ASSEMBLY_USAGE_OCCURRENCE ( 'NAUO8', ' ', ' ', #16665, #15789, $ ) ;
#17976 = NEXT_ASSEMBLY_USAGE_OCCURRENCE ( 'NAUO9', ' ', ' ', #16665, #12337, $ ) ;
#17977 = NEXT_ASSEMBLY_USAGE_OCCURRENCE ( 'NAUO10', ' ', ' ', #16665, #14992, $ ) ;
#17978 = NEXT_ASSEMBLY_USAGE_OCCURRENCE ( 'NAUO11', ' ', ' ', #16665, #12337, $ ) ;
#17979 = NEXT_ASSEMBLY_USAGE_OCCURRENCE ( 'NAUO12', ' ', ' ', #16665, #5901, $ ) ;
#17980 = NEXT_ASSEMBLY_USAGE_OCCURRENCE ( 'NAUO13', ' ', ' ', #16665, #817, $ ) ;
#17981 = NEXT_ASSEMBLY_USAGE_OCCURRENCE ( 'NAUO14', ' ', ' ', #16665, #817, $ ) ;
#17982 = NEXT_ASSEMBLY_USAGE_OCCURRENCE ( 'NAUO15', ' ', ' ', #16665, #817, $ ) ;
#17983 = NEXT_ASSEMBLY_USAGE_OCCURRENCE ( 'NAUO16', ' ', ' ', #16665, #15223, $ ) ;
#17984 = NEXT_ASSEMBLY_USAGE_OCCURRENCE ( 'NAUO17', ' ', ' ', #16665, #15223, $ ) ;
#17985 = NEXT_ASSEMBLY_USAGE_OCCURRENCE ( 'NAUO18', ' ', ' ', #16665, #15223, $ ) ;
ENDSEC;
END-ISO-10303-21;
